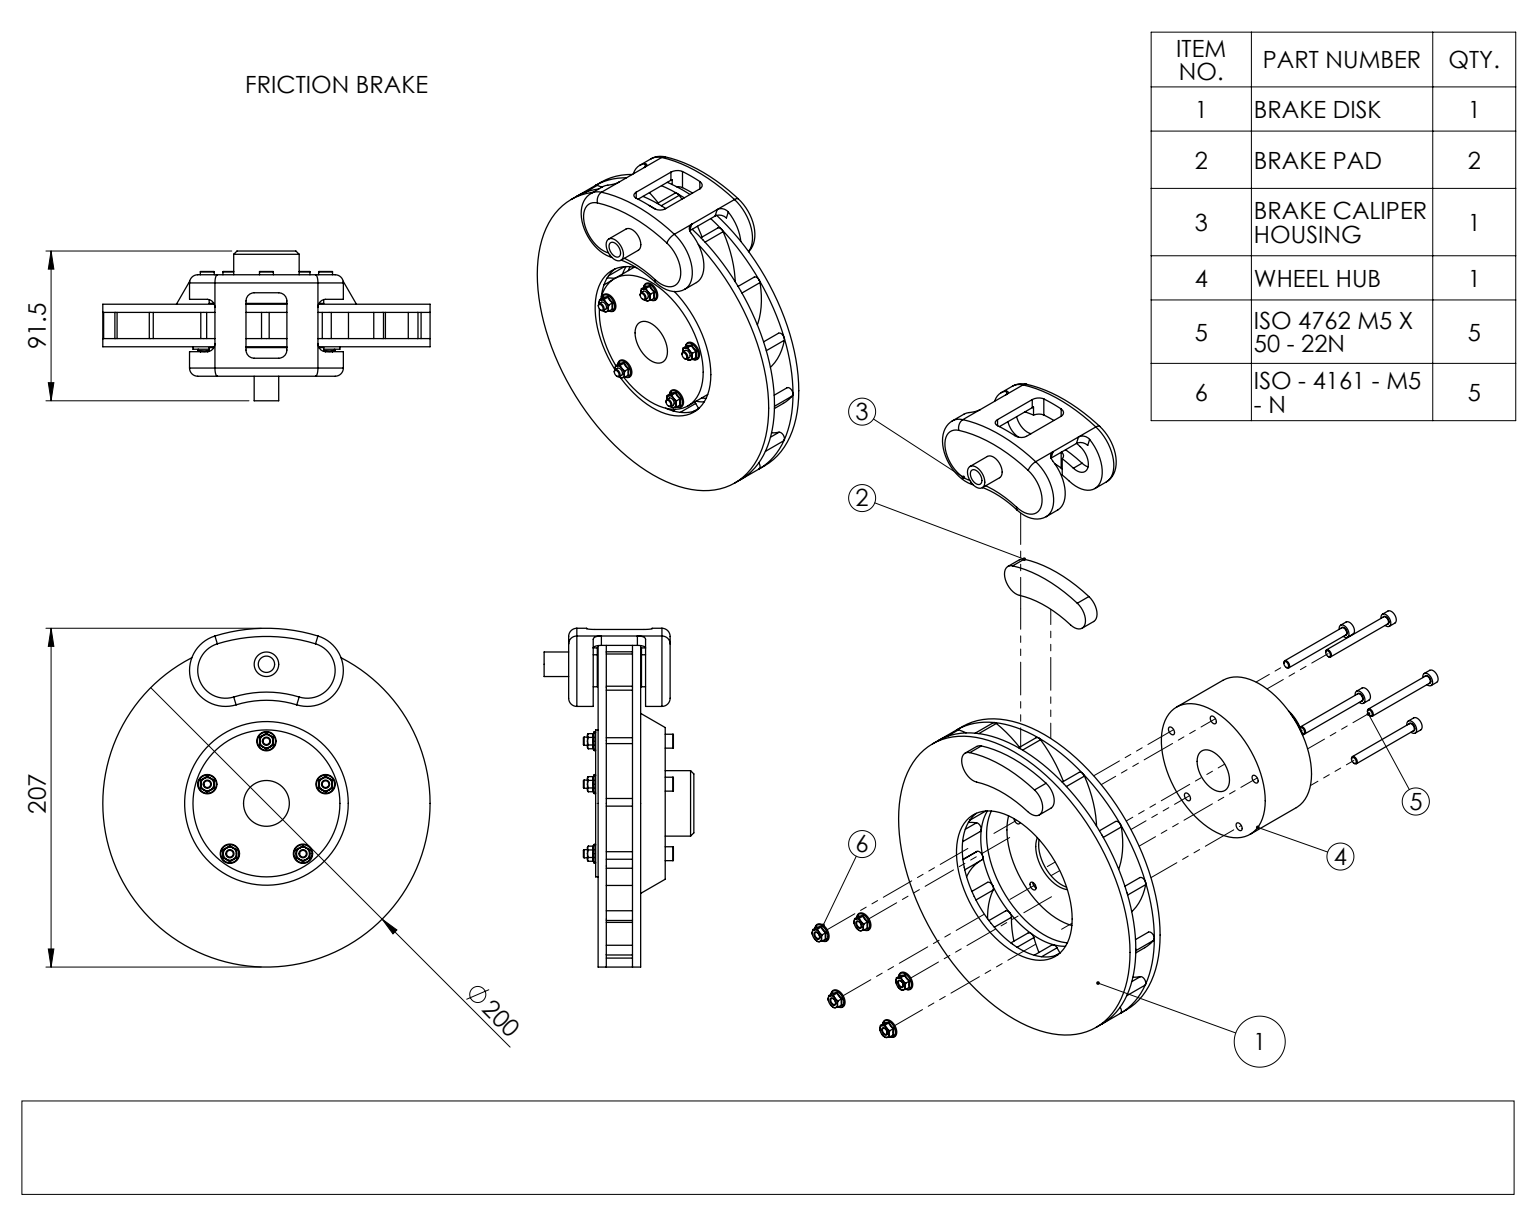
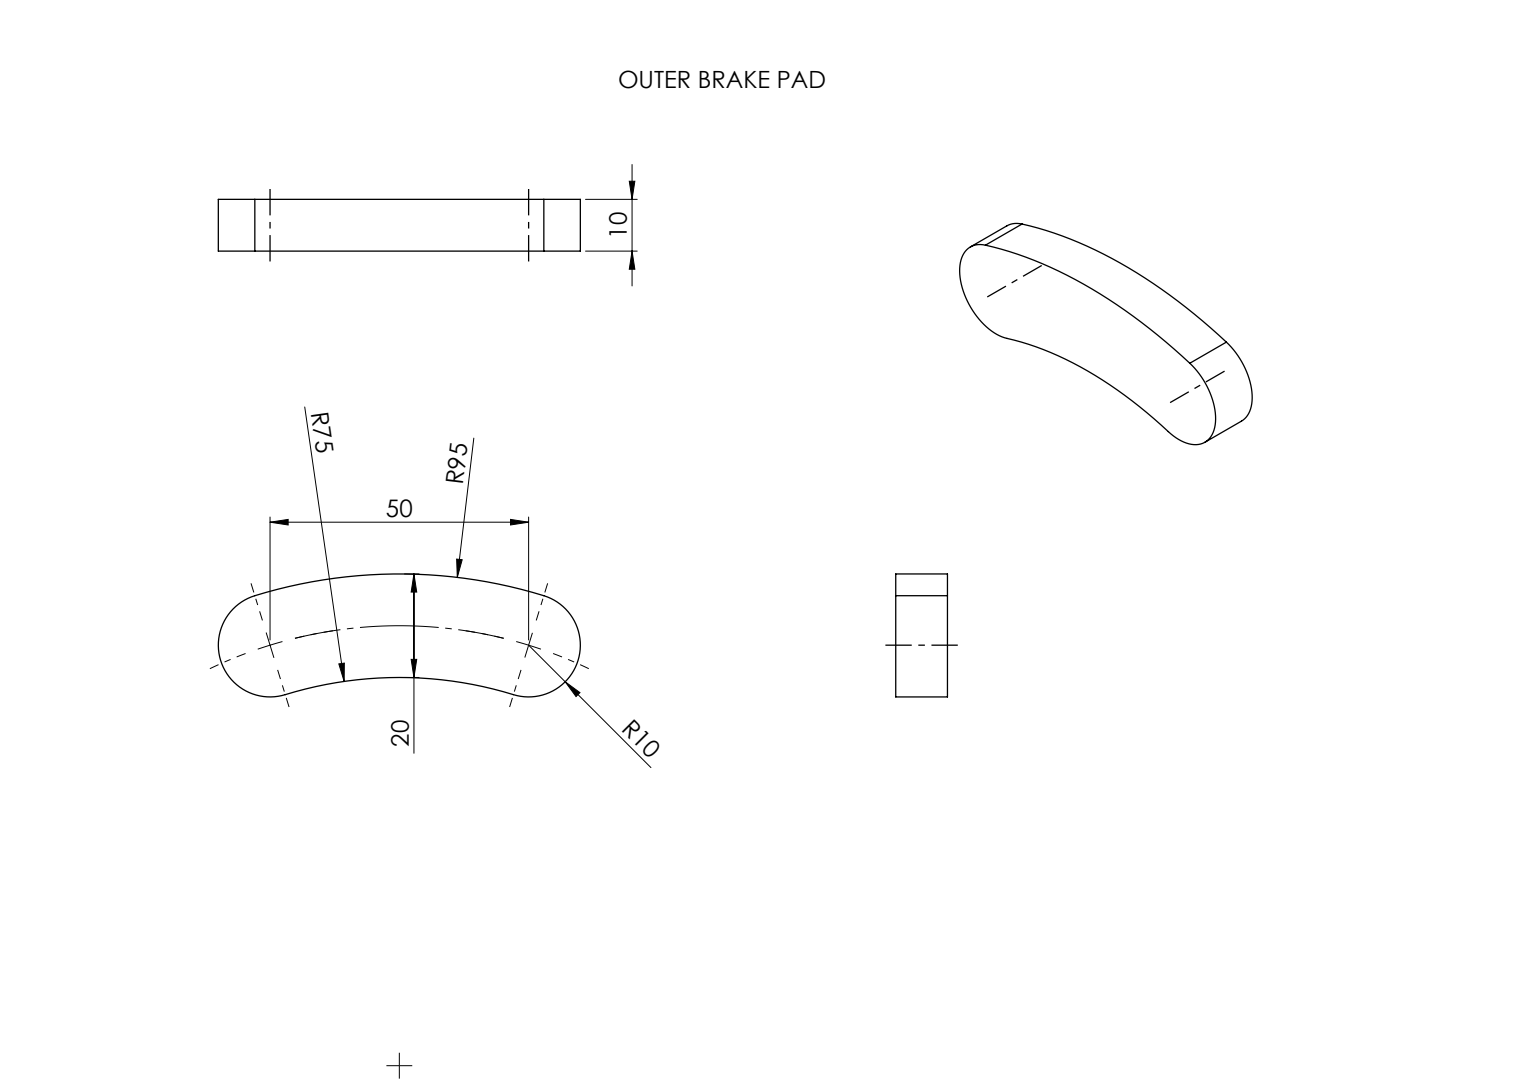
ISO-10303-21;
HEADER;
FILE_DESCRIPTION (('STEP AP214'),
    '1' );
FILE_NAME ('BR-595',
    '2026-10-02T06:35:35',
    ( '' ),
    ( '' ),
    'SwSTEP 2.0',
    'SolidWorks 2026',
    '' );
FILE_SCHEMA (( 'AUTOMOTIVE_DESIGN' ));
ENDSEC;

DATA;
#1 = ORIENTED_EDGE ( 'NONE', *, *, #7352, .F. ) ;
#2 = DIRECTION ( 'NONE',  ( -1.000000000000000000, 0.000000000000000000, 0.000000000000000000 ) ) ;
#3 = DIRECTION ( 'NONE',  ( -1.000000000000000000, 0.000000000000000000, 0.000000000000000000 ) ) ;
#4 = ORIENTED_EDGE ( 'NONE', *, *, #5380, .F. ) ;
#5 = DIRECTION ( 'NONE',  ( -1.000000000000000000, 0.000000000000000000, 0.000000000000000000 ) ) ;
#6 = CIRCLE ( 'NONE', #12861, 63.00000000000000000 ) ;
#7 = CARTESIAN_POINT ( 'NONE',  ( 53.06332297728253877, -7.252293700256950082, -10.50000000000000000 ) ) ;
#8 = FACE_OUTER_BOUND ( 'NONE', #11130, .T. ) ;
#9 = CARTESIAN_POINT ( 'NONE',  ( 2.500000000000002220, -1.178949249685208533, 2.042000000000002036 ) ) ;
#10 = CIRCLE ( 'NONE', #12379, 59.50000000000000711 ) ;
#11 = CARTESIAN_POINT ( 'NONE',  ( 0.000000000000000000, 0.000000000000000000, -10.50000000000000000 ) ) ;
#12 = AXIS2_PLACEMENT_3D ( 'NONE', #10324, #12760, #3495 ) ;
#13 = DIRECTION ( 'NONE',  ( -1.000000000000000000, 0.000000000000000000, 0.000000000000000000 ) ) ;
#14 = VERTEX_POINT ( 'NONE', #5600 ) ;
#15 = AXIS2_PLACEMENT_3D ( 'NONE', #1974, #14669, #772 ) ;
#16 = CARTESIAN_POINT ( 'NONE',  ( -9.706953719245875689, -57.06275842387046993, 10.49999999999999822 ) ) ;
#17 = CARTESIAN_POINT ( 'NONE',  ( 54.55500000000000682, 0.000000000000000000, 0.000000000000000000 ) ) ;
#18 = AXIS2_PLACEMENT_3D ( 'NONE', #11160, #14736, #14806 ) ;
#19 = DIRECTION ( 'NONE',  ( 0.000000000000000000, 0.000000000000000000, 1.000000000000000000 ) ) ;
#20 = CIRCLE ( 'NONE', #4639, 50.00000000000000000 ) ;
#21 = CARTESIAN_POINT ( 'NONE',  ( -3.999999999999996447, 0.000000000000000000, 0.000000000000000000 ) ) ;
#22 = AXIS2_PLACEMENT_3D ( 'NONE', #10002, #1881, #9007 ) ;
#23 = VERTEX_POINT ( 'NONE', #4041 ) ;
#24 = ADVANCED_FACE ( 'NONE', ( #13370 ), #10311, .T. ) ;
#25 = CARTESIAN_POINT ( 'NONE',  ( -57.06275842387042729, 9.706953719246069312, 10.49999999999999822 ) ) ;
#26 = ADVANCED_FACE ( 'NONE', ( #7589 ), #2370, .T. ) ;
#27 = VERTEX_POINT ( 'NONE', #8027 ) ;
#28 = CARTESIAN_POINT ( 'NONE',  ( 0.000000000000000000, 0.000000000000000000, -43.49999999999998579 ) ) ;
#29 = DIRECTION ( 'NONE',  ( 1.000000000000000000, 0.000000000000000000, 0.000000000000000000 ) ) ;
#30 = AXIS2_PLACEMENT_3D ( 'NONE', #3946, #7114, #5981 ) ;
#31 = DIRECTION ( 'NONE',  ( 1.000000000000000000, 0.000000000000000000, 0.000000000000000000 ) ) ;
#32 = DIRECTION ( 'NONE',  ( -1.000000000000000000, 0.000000000000000000, 0.000000000000000000 ) ) ;
#33 = AXIS2_PLACEMENT_3D ( 'NONE', #14453, #639, #4058 ) ;
#34 = EDGE_LOOP ( 'NONE', ( #1936, #8130, #14973, #10499, #11470, #9709, #14107 ) ) ;
#35 = AXIS2_PLACEMENT_3D ( 'NONE', #9136, #13779, #7988 ) ;
#36 = DIRECTION ( 'NONE',  ( -0.000000000000000000, -0.000000000000000000, -1.000000000000000000 ) ) ;
#37 = CYLINDRICAL_SURFACE ( 'NONE', #355, 22.00000000000001421 ) ;
#38 = DIRECTION ( 'NONE',  ( -0.000000000000000000, -0.000000000000000000, -1.000000000000000000 ) ) ;
#39 = ORIENTED_EDGE ( 'NONE', *, *, #13925, .F. ) ;
#40 = AXIS2_PLACEMENT_3D ( 'NONE', #3441, #1165, #12924 ) ;
#41 = EDGE_LOOP ( 'NONE', ( #8481, #11440, #8445, #13506, #14760, #3452, #6224, #9398, #1796 ) ) ;
#42 = EDGE_CURVE ( 'NONE', #5654, #12729, #7938, .T. ) ;
#43 = EDGE_CURVE ( 'NONE', #8906, #2094, #9864, .T. ) ;
#44 = ORIENTED_EDGE ( 'NONE', *, *, #3478, .T. ) ;
#45 = AXIS2_PLACEMENT_3D ( 'NONE', #573, #4845, #14470 ) ;
#46 = CYLINDRICAL_SURFACE ( 'NONE', #4967, 3.000000000000002665 ) ;
#47 = CARTESIAN_POINT ( 'NONE',  ( 47.00000000000001421, 81.24038404635960831, -31.00000000000000000 ) ) ;
#48 = FACE_BOUND ( 'NONE', #7708, .T. ) ;
#49 = CARTESIAN_POINT ( 'NONE',  ( 36.14014761921570340, 11.74264578624841171, -25.50000000000000355 ) ) ;
#50 = DIRECTION ( 'NONE',  ( 0.000000000000000000, 0.000000000000000000, 1.000000000000000000 ) ) ;
#51 = EDGE_LOOP ( 'NONE', ( #11368, #1318, #14890, #12577, #3403 ) ) ;
#52 = CARTESIAN_POINT ( 'NONE',  ( 36.08010649850015739, 100.2464683348682541, -16.00000000000000000 ) ) ;
#53 = DIRECTION ( 'NONE',  ( 1.000000000000000000, 0.000000000000000000, 0.000000000000000000 ) ) ;
#54 = AXIS2_PLACEMENT_3D ( 'NONE', #13528, #11036, #940 ) ;
#55 = ORIENTED_EDGE ( 'NONE', *, *, #8567, .F. ) ;
#56 = ORIENTED_EDGE ( 'NONE', *, *, #8508, .F. ) ;
#57 = DIRECTION ( 'NONE',  ( 0.000000000000000000, 0.000000000000000000, 1.000000000000000000 ) ) ;
#58 = ORIENTED_EDGE ( 'NONE', *, *, #13027, .F. ) ;
#59 = AXIS2_PLACEMENT_3D ( 'NONE', #11530, #114, #4460 ) ;
#60 = CARTESIAN_POINT ( 'NONE',  ( -69.16568774265545017, 71.53347797788843820, -13.00000000000000178 ) ) ;
#61 = CARTESIAN_POINT ( 'NONE',  ( 0.000000000000000000, 0.000000000000000000, -10.50000000000000000 ) ) ;
#62 = EDGE_CURVE ( 'NONE', #7405, #1485, #13775, .T. ) ;
#63 = AXIS2_PLACEMENT_3D ( 'NONE', #8204, #12550, #5924 ) ;
#64 = CARTESIAN_POINT ( 'NONE',  ( 0.000000000000000000, 4.618802153517009401, -0.5000000000000004441 ) ) ;
#65 = CARTESIAN_POINT ( 'NONE',  ( 0.000000000000000000, 0.000000000000000000, -13.00000000000000178 ) ) ;
#66 = VECTOR ( 'NONE', #7777, 1000.000000000000000 ) ;
#67 = CARTESIAN_POINT ( 'NONE',  ( 66.70695371924546180, 57.06275842387054098, 8.000000000000000000 ) ) ;
#68 = CARTESIAN_POINT ( 'NONE',  ( 50.84834283436990177, 14.07862063237912054, -13.00000000000000178 ) ) ;
#69 = ADVANCED_FACE ( 'NONE', ( #14874 ), #12670, .F. ) ;
#70 = ORIENTED_EDGE ( 'NONE', *, *, #7162, .T. ) ;
#71 = CARTESIAN_POINT ( 'NONE',  ( 0.000000000000000000, 4.618802153517009401, -3.433295621305381573 ) ) ;
#72 = AXIS2_PLACEMENT_3D ( 'NONE', #14916, #10416, #5859 ) ;
#73 = EDGE_CURVE ( 'NONE', #4839, #9064, #14954, .T. ) ;
#74 = LINE ( 'NONE', #12542, #3120 ) ;
#75 = ORIENTED_EDGE ( 'NONE', *, *, #14051, .F. ) ;
#76 = FILL_AREA_STYLE ('',( #3580 ) ) ;
#77 = AXIS2_PLACEMENT_3D ( 'NONE', #3248, #7868, #12355 ) ;
#78 = DIRECTION ( 'NONE',  ( 1.000000000000000000, 0.000000000000000000, 0.000000000000000000 ) ) ;
#79 = EDGE_LOOP ( 'NONE', ( #12586, #8672, #6412, #11812, #13520, #7331 ) ) ;
#80 = CYLINDRICAL_SURFACE ( 'NONE', #13351, 59.50000000000000000 ) ;
#81 = EDGE_CURVE ( 'NONE', #7416, #8383, #7204, .T. ) ;
#82 = CIRCLE ( 'NONE', #4216, 63.00000000000000000 ) ;
#83 = EDGE_CURVE ( 'NONE', #7502, #10004, #12318, .T. ) ;
#84 = DIRECTION ( 'NONE',  ( 0.000000000000000000, 0.000000000000000000, 1.000000000000000000 ) ) ;
#85 = CYLINDRICAL_SURFACE ( 'NONE', #14315, 56.99999999999999289 ) ;
#86 = LINE ( 'NONE', #9270, #8545 ) ;
#87 = CARTESIAN_POINT ( 'NONE',  ( -3.999999999999999112, 2.471528634177587946, -3.686887442155188932 ) ) ;
#88 = FACE_OUTER_BOUND ( 'NONE', #3167, .T. ) ;
#89 = CIRCLE ( 'NONE', #12700, 0.2000000000000000944 ) ;
#90 = ORIENTED_EDGE ( 'NONE', *, *, #1930, .F. ) ;
#91 = EDGE_CURVE ( 'NONE', #7570, #11525, #4401, .T. ) ;
#92 = CARTESIAN_POINT ( 'NONE',  ( -10.00610186947451474, 106.5314655734664910, -19.33904518629106306 ) ) ;
#93 = CARTESIAN_POINT ( 'NONE',  ( -2.344047193898592063, -3.265465875126478679, -8.534280460060699911E-15 ) ) ;
#94 = B_SPLINE_CURVE_WITH_KNOTS ( 'NONE', 3,
 ( #9442, #2468, #4910, #4826, #14091, #9801, #11106, #8665, #3618, #8738, #13380, #3696, #12955, #2552, #2981, #7235, #10661, #9522, #3776, #4761 ),
 .UNSPECIFIED., .F., .F.,
 ( 4, 2, 2, 2, 2, 2, 2, 2, 2, 4 ),
 ( 0.000000000000000000, 0.0009783709435495714819, 0.001467556415324351151, 0.001956741887099130821, 0.002935112830648695798, 0.003913483774198260774, 0.004891854717747825751, 0.005870225661297390728, 0.006848596604846954837, 0.007826967548396519814 ),
 .UNSPECIFIED. ) ;
#95 = DIRECTION ( 'NONE',  ( 1.000000000000000000, 0.000000000000000000, 0.000000000000000000 ) ) ;
#96 = DIRECTION ( 'NONE',  ( 0.000000000000000000, 0.000000000000000000, -1.000000000000000000 ) ) ;
#97 = ORIENTED_EDGE ( 'NONE', *, *, #2089, .T. ) ;
#98 = CIRCLE ( 'NONE', #1556, 2.649999999999992806 ) ;
#99 = AXIS2_PLACEMENT_3D ( 'NONE', #4932, #13204, #7338 ) ;
#100 = FACE_OUTER_BOUND ( 'NONE', #3263, .T. ) ;
#101 = AXIS2_PLACEMENT_3D ( 'NONE', #2141, #150, #5905 ) ;
#102 = ORIENTED_EDGE ( 'NONE', *, *, #4360, .F. ) ;
#103 = DIRECTION ( 'NONE',  ( -1.000000000000000000, 0.000000000000000000, 0.000000000000000000 ) ) ;
#104 = DIRECTION ( 'NONE',  ( 1.000000000000000000, 0.000000000000000000, 0.000000000000000000 ) ) ;
#105 = PLANE ( 'NONE',  #6564 ) ;
#106 = DIRECTION ( 'NONE',  ( -0.000000000000000000, -0.000000000000000000, 1.000000000000000000 ) ) ;
#107 = VECTOR ( 'NONE', #12064, 1000.000000000000000 ) ;
#108 = EDGE_LOOP ( 'NONE', ( #5288, #10008 ) ) ;
#109 = CIRCLE ( 'NONE', #11524, 3.000000000000004441 ) ;
#110 = AXIS2_PLACEMENT_3D ( 'NONE', #13113, #9527, #4007 ) ;
#111 = DIRECTION ( 'NONE',  ( 1.000000000000000000, 0.000000000000000000, 0.000000000000000000 ) ) ;
#112 = DIRECTION ( 'NONE',  ( 0.000000000000000000, 0.000000000000000000, -1.000000000000000000 ) ) ;
#113 = AXIS2_PLACEMENT_3D ( 'NONE', #5450, #3170, #7481 ) ;
#114 = DIRECTION ( 'NONE',  ( -0.000000000000000000, -0.000000000000000000, -1.000000000000000000 ) ) ;
#115 = ORIENTED_EDGE ( 'NONE', *, *, #13152, .T. ) ;
#116 = ORIENTED_EDGE ( 'NONE', *, *, #9973, .T. ) ;
#117 = STYLED_ITEM ( 'NONE', ( #11100 ), #4169 ) ;
#118 = ORIENTED_EDGE ( 'NONE', *, *, #6384, .T. ) ;
#119 = AXIS2_PLACEMENT_3D ( 'NONE', #2152, #13621, #8984 ) ;
#120 = DIRECTION ( 'NONE',  ( -1.000000000000000000, 0.000000000000000000, 0.000000000000000000 ) ) ;
#121 = AXIS2_PLACEMENT_3D ( 'NONE', #1011, #8960, #6603 ) ;
#122 = FACE_OUTER_BOUND ( 'NONE', #11782, .T. ) ;
#123 = CARTESIAN_POINT ( 'NONE',  ( 2.836893136758667833, 3.208949435746013545, -3.505054077164964976 ) ) ;
#124 = CARTESIAN_POINT ( 'NONE',  ( 7.417888187663120192, 52.54657765281190507, -13.00000000000000178 ) ) ;
#125 = EDGE_CURVE ( 'NONE', #6463, #5657, #11381, .T. ) ;
#126 = ORIENTED_EDGE ( 'NONE', *, *, #9552, .T. ) ;
#127 = CARTESIAN_POINT ( 'NONE',  ( -10.20439220990035345, 94.45068983291282905, 19.21516791372541633 ) ) ;
#128 = ORIENTED_EDGE ( 'NONE', *, *, #10022, .F. ) ;
#129 = ADVANCED_FACE ( 'NONE', ( #13654 ), #8723, .F. ) ;
#130 = ORIENTED_EDGE ( 'NONE', *, *, #424, .F. ) ;
#131 = EDGE_CURVE ( 'NONE', #9943, #5635, #9786, .T. ) ;
#132 = VERTEX_POINT ( 'NONE', #14438 ) ;
#133 = EDGE_CURVE ( 'NONE', #4919, #1677, #14989, .T. ) ;
#134 = CARTESIAN_POINT ( 'NONE',  ( 4.154306624730861763, 2.398490048084776394, -3.721999068284301604 ) ) ;
#135 = CARTESIAN_POINT ( 'NONE',  ( 12.50000000000000000, 40.62019202317980415, -16.00000000000000000 ) ) ;
#136 = CIRCLE ( 'NONE', #11783, 63.00000000000000000 ) ;
#137 = CARTESIAN_POINT ( 'NONE',  ( 10.21169758550232309, 62.16852661215632025, 19.23993411931846254 ) ) ;
#138 = ORIENTED_EDGE ( 'NONE', *, *, #8514, .T. ) ;
#139 = CIRCLE ( 'NONE', #6147, 3.000000000000002665 ) ;
#140 = EDGE_LOOP ( 'NONE', ( #7272, #903, #5586, #9223, #6785, #6818 ) ) ;
#141 = DIRECTION ( 'NONE',  ( -0.000000000000000000, -0.000000000000000000, -1.000000000000000000 ) ) ;
#142 = EDGE_CURVE ( 'NONE', #2335, #4523, #8651, .T. ) ;
#143 = VERTEX_POINT ( 'NONE', #12163 ) ;
#144 = VECTOR ( 'NONE', #4829, 1000.000000000000000 ) ;
#145 = DIRECTION ( 'NONE',  ( -0.000000000000000000, -0.000000000000000000, 1.000000000000000000 ) ) ;
#146 = DIRECTION ( 'NONE',  ( -1.000000000000000000, 0.000000000000000000, 0.000000000000000000 ) ) ;
#147 = CIRCLE ( 'NONE', #10081, 0.5000000000000004441 ) ;
#148 = DIRECTION ( 'NONE',  ( 1.000000000000000000, 0.000000000000000000, 0.000000000000000000 ) ) ;
#149 = SURFACE_STYLE_FILL_AREA ( #5069 ) ;
#150 = DIRECTION ( 'NONE',  ( -0.000000000000000000, -0.000000000000000000, 1.000000000000000000 ) ) ;
#151 = DIRECTION ( 'NONE',  ( 0.000000000000000000, 0.000000000000000000, 1.000000000000000000 ) ) ;
#152 = ORIENTED_EDGE ( 'NONE', *, *, #3887, .F. ) ;
#153 = DIRECTION ( 'NONE',  ( -1.000000000000000000, 0.000000000000000000, 0.000000000000000000 ) ) ;
#154 = CIRCLE ( 'NONE', #13005, 2.649999999999985700 ) ;
#155 = ADVANCED_FACE ( 'NONE', ( #11017 ), #623, .F. ) ;
#156 = ORIENTED_EDGE ( 'NONE', *, *, #4969, .T. ) ;
#157 =( NAMED_UNIT ( * ) SI_UNIT ( $, .STERADIAN. ) SOLID_ANGLE_UNIT ( ) );
#158 = ORIENTED_EDGE ( 'NONE', *, *, #13672, .T. ) ;
#159 = CARTESIAN_POINT ( 'NONE',  ( 2.500000000000002220, 0.000000000000000000, 0.000000000000000000 ) ) ;
#160 = ORIENTED_EDGE ( 'NONE', *, *, #4028, .F. ) ;
#161 = CARTESIAN_POINT ( 'NONE',  ( 2.500000000000002220, -1.178949249685208533, 2.042000000000002036 ) ) ;
#162 = CARTESIAN_POINT ( 'NONE',  ( -52.72775723226775568, 7.383907457638128058, -13.00000000000000178 ) ) ;
#163 = DIRECTION ( 'NONE',  ( 1.000000000000000000, 0.000000000000000000, 0.000000000000000000 ) ) ;
#164 = CARTESIAN_POINT ( 'NONE',  ( -53.63365512954686665, 9.714003807514082212, 8.000000000000000000 ) ) ;
#165 = AXIS2_PLACEMENT_3D ( 'NONE', #7612, #12181, #14531 ) ;
#166 = DIRECTION ( 'NONE',  ( -0.000000000000000000, -0.000000000000000000, -1.000000000000000000 ) ) ;
#167 = CARTESIAN_POINT ( 'NONE',  ( 36.14014761921570340, 11.74264578624841171, -28.00000000000000000 ) ) ;
#168 = ORIENTED_EDGE ( 'NONE', *, *, #2760, .F. ) ;
#169 = CARTESIAN_POINT ( 'NONE',  ( 0.000000000000000000, 0.000000000000000000, -10.50000000000000000 ) ) ;
#170 = DIRECTION ( 'NONE',  ( 1.000000000000000000, 0.000000000000000000, 0.000000000000000000 ) ) ;
#171 = EDGE_CURVE ( 'NONE', #8488, #2518, #8671, .T. ) ;
#172 = EDGE_CURVE ( 'NONE', #8464, #345, #2401, .T. ) ;
#173 = FACE_OUTER_BOUND ( 'NONE', #9202, .T. ) ;
#174 = CARTESIAN_POINT ( 'NONE',  ( 33.48561063518626923, -47.21331623427104063, 10.49999999999999822 ) ) ;
#175 = ORIENTED_EDGE ( 'NONE', *, *, #2159, .T. ) ;
#176 = CARTESIAN_POINT ( 'NONE',  ( -45.96504489225991819, 23.50071946824089153, -8.000000000000000000 ) ) ;
#177 = ORIENTED_EDGE ( 'NONE', *, *, #5197, .F. ) ;
#178 = DIRECTION ( 'NONE',  ( 1.000000000000000000, 0.000000000000000000, -0.000000000000000000 ) ) ;
#179 = CARTESIAN_POINT ( 'NONE',  ( 35.00000000000000000, 81.24038404635960831, 16.00000000000000000 ) ) ;
#180 = EDGE_CURVE ( 'NONE', #2333, #2935, #11831, .T. ) ;
#181 = CARTESIAN_POINT ( 'NONE',  ( 70.71067811865488295, 70.71067811865464137, 8.000000000000000000 ) ) ;
#182 = DIRECTION ( 'NONE',  ( -0.000000000000000000, -0.000000000000000000, -1.000000000000000000 ) ) ;
#183 = ORIENTED_EDGE ( 'NONE', *, *, #10022, .T. ) ;
#184 = PLANE ( 'NONE',  #4038 ) ;
#185 = DIRECTION ( 'NONE',  ( 1.000000000000000000, 0.000000000000000000, 0.000000000000000000 ) ) ;
#186 = ADVANCED_FACE ( 'NONE', ( #285 ), #5969, .F. ) ;
#187 = DIRECTION ( 'NONE',  ( 0.000000000000000000, 0.000000000000000000, -1.000000000000000000 ) ) ;
#188 = ORIENTED_EDGE ( 'NONE', *, *, #4452, .F. ) ;
#189 = ORIENTED_EDGE ( 'NONE', *, *, #647, .F. ) ;
#190 = ORIENTED_EDGE ( 'NONE', *, *, #13352, .T. ) ;
#191 = DIRECTION ( 'NONE',  ( -0.000000000000000000, -0.000000000000000000, -1.000000000000000000 ) ) ;
#192 = DIRECTION ( 'NONE',  ( -0.000000000000000000, -0.000000000000000000, 1.000000000000000000 ) ) ;
#193 = DIRECTION ( 'NONE',  ( 0.000000000000000000, 0.000000000000000000, 1.000000000000000000 ) ) ;
#194 = SURFACE_SIDE_STYLE ('',( #3699 ) ) ;
#195 = CARTESIAN_POINT ( 'NONE',  ( 92.61631465359491244, 37.12029293941346708, -13.00000000000000178 ) ) ;
#196 = ORIENTED_EDGE ( 'NONE', *, *, #12416, .F. ) ;
#197 = VERTEX_POINT ( 'NONE', #8248 ) ;
#198 = VERTEX_POINT ( 'NONE', #2479 ) ;
#199 = CARTESIAN_POINT ( 'NONE',  ( 43.30127018922200222, -24.99999999999988276, -8.000000000000000000 ) ) ;
#200 = DIRECTION ( 'NONE',  ( 0.000000000000000000, 0.000000000000000000, -1.000000000000000000 ) ) ;
#201 = CARTESIAN_POINT ( 'NONE',  ( 11.10302805179279240, 62.01554028455485224, 18.51404809149990882 ) ) ;
#202 = ORIENTED_EDGE ( 'NONE', *, *, #1757, .T. ) ;
#203 = VERTEX_POINT ( 'NONE', #9455 ) ;
#204 = DIRECTION ( 'NONE',  ( -0.000000000000000000, -0.000000000000000000, -1.000000000000000000 ) ) ;
#205 = ORIENTED_EDGE ( 'NONE', *, *, #9389, .F. ) ;
#206 = EDGE_CURVE ( 'NONE', #7611, #11559, #11845, .T. ) ;
#207 = CARTESIAN_POINT ( 'NONE',  ( -57.06275842387042729, 9.706953719246069312, -8.000000000000000000 ) ) ;
#208 = DIRECTION ( 'NONE',  ( -1.000000000000000000, 0.000000000000000000, 0.000000000000000000 ) ) ;
#209 = ADVANCED_FACE ( 'NONE', ( #8178 ), #13040, .T. ) ;
#210 = CARTESIAN_POINT ( 'NONE',  ( 0.2500000000000002220, 0.000000000000000000, 4.250000000000000000 ) ) ;
#211 = DIRECTION ( 'NONE',  ( 0.000000000000000000, 0.000000000000000000, -1.000000000000000000 ) ) ;
#212 = VERTEX_POINT ( 'NONE', #10456 ) ;
#213 = LINE ( 'NONE', #4355, #3743 ) ;
#214 = CARTESIAN_POINT ( 'NONE',  ( -89.89283556784485540, 37.53686968382331202, 10.49999999999999822 ) ) ;
#215 = VERTEX_POINT ( 'NONE', #4771 ) ;
#216 = DIRECTION ( 'NONE',  ( 0.000000000000000000, 1.000000000000000000, 0.000000000000000000 ) ) ;
#217 = ORIENTED_EDGE ( 'NONE', *, *, #892, .F. ) ;
#218 = VERTEX_POINT ( 'NONE', #1279 ) ;
#219 = VERTEX_POINT ( 'NONE', #12746 ) ;
#220 = ADVANCED_FACE ( 'NONE', ( #7246 ), #8324, .F. ) ;
#221 = DIRECTION ( 'NONE',  ( 0.000000000000000000, 0.000000000000000000, -1.000000000000000000 ) ) ;
#222 = AXIS2_PLACEMENT_3D ( 'NONE', #233, #10789, #392 ) ;
#223 = CARTESIAN_POINT ( 'NONE',  ( 25.00000000000000000, 81.24038404635960831, 26.00000000000000000 ) ) ;
#224 = EDGE_LOOP ( 'NONE', ( #11298, #11985, #10533, #2386, #7022, #5370 ) ) ;
#225 = EDGE_CURVE ( 'NONE', #11976, #1441, #7021, .T. ) ;
#226 = ORIENTED_EDGE ( 'NONE', *, *, #3230, .T. ) ;
#227 = CARTESIAN_POINT ( 'NONE',  ( 3.999999999999996447, -2.309401076758518911, -3.433295621305385126 ) ) ;
#228 = CARTESIAN_POINT ( 'NONE',  ( 0.000000000000000000, 0.000000000000000000, 10.50000000000000000 ) ) ;
#229 = DIRECTION ( 'NONE',  ( -0.000000000000000000, -0.000000000000000000, 1.000000000000000000 ) ) ;
#230 = CARTESIAN_POINT ( 'NONE',  ( 12.39897948556635754, 61.76783392443436327, 16.00000000000000000 ) ) ;
#231 = AXIS2_PLACEMENT_3D ( 'NONE', #12118, #6402, #3087 ) ;
#232 = CIRCLE ( 'NONE', #11153, 59.50000000000000000 ) ;
#233 = CARTESIAN_POINT ( 'NONE',  ( 6.917888187663118416, 52.54657765281190507, -13.00000000000000178 ) ) ;
#234 = EDGE_LOOP ( 'NONE', ( #1184, #579, #7849, #6661 ) ) ;
#235 = CIRCLE ( 'NONE', #7737, 3.000000000000002665 ) ;
#236 = DIRECTION ( 'NONE',  ( 0.000000000000000000, 0.000000000000000000, -1.000000000000000000 ) ) ;
#237 = ORIENTED_EDGE ( 'NONE', *, *, #10239, .T. ) ;
#238 = VECTOR ( 'NONE', #6357, 1000.000000000000000 ) ;
#239 = CARTESIAN_POINT ( 'NONE',  ( 0.000000000000000000, 0.000000000000000000, -13.00000000000000178 ) ) ;
#240 = CYLINDRICAL_SURFACE ( 'NONE', #5888, 0.5000000000000004441 ) ;
#241 = DIRECTION ( 'NONE',  ( 0.000000000000000000, 0.000000000000000000, 1.000000000000000000 ) ) ;
#242 = AXIS2_PLACEMENT_3D ( 'NONE', #11255, #4428, #1840 ) ;
#243 = B_SPLINE_CURVE_WITH_KNOTS ( 'NONE', 3,
 ( #4332, #3259, #11468, #1065, #15025, #13745 ),
 .UNSPECIFIED., .F., .F.,
 ( 4, 2, 4 ),
 ( -3.640115492410820263E-06, 0.0002066546034003392330, 0.0004169493222930892523 ),
 .UNSPECIFIED. ) ;
#244 = DIRECTION ( 'NONE',  ( 0.000000000000000000, 0.000000000000000000, 1.000000000000000000 ) ) ;
#245 = EDGE_LOOP ( 'NONE', ( #12911, #1425, #6697, #4365 ) ) ;
#246 = VECTOR ( 'NONE', #11341, 1000.000000000000000 ) ;
#247 = CARTESIAN_POINT ( 'NONE',  ( 0.000000000000000000, 0.000000000000000000, -13.00000000000000178 ) ) ;
#248 = AXIS2_PLACEMENT_3D ( 'NONE', #2313, #11658, #11591 ) ;
#249 = EDGE_LOOP ( 'NONE', ( #12812, #11025, #8242, #14279, #562, #14719, #2020, #11276, #2397 ) ) ;
#250 = DIRECTION ( 'NONE',  ( -0.000000000000000000, -0.000000000000000000, 1.000000000000000000 ) ) ;
#251 = DIRECTION ( 'NONE',  ( 0.000000000000000000, 0.000000000000000000, -1.000000000000000000 ) ) ;
#252 = EDGE_CURVE ( 'NONE', #915, #5997, #13054, .T. ) ;
#253 = FACE_OUTER_BOUND ( 'NONE', #11246, .T. ) ;
#254 = EDGE_CURVE ( 'NONE', #13058, #12937, #12889, .T. ) ;
#255 = DIRECTION ( 'NONE',  ( 0.000000000000000000, 0.000000000000000000, -1.000000000000000000 ) ) ;
#256 = CIRCLE ( 'NONE', #11911, 100.0000000000000000 ) ;
#257 = AXIS2_PLACEMENT_3D ( 'NONE', #4931, #14259, #10909 ) ;
#258 = ORIENTED_EDGE ( 'NONE', *, *, #4361, .T. ) ;
#259 = VERTEX_POINT ( 'NONE', #10384 ) ;
#260 = PLANE ( 'NONE',  #2332 ) ;
#261 = VECTOR ( 'NONE', #10408, 1000.000000000000000 ) ;
#262 = LINE ( 'NONE', #9512, #1094 ) ;
#263 = AXIS2_PLACEMENT_3D ( 'NONE', #3425, #1153, #13759 ) ;
#264 = CIRCLE ( 'NONE', #5603, 100.0000000000000000 ) ;
#265 = CARTESIAN_POINT ( 'NONE',  ( 2.500000000000002220, -2.357898499370437939, 0.000000000000000000 ) ) ;
#266 = EDGE_CURVE ( 'NONE', #4701, #13246, #688, .T. ) ;
#267 = ORIENTED_EDGE ( 'NONE', *, *, #14506, .F. ) ;
#268 = AXIS2_PLACEMENT_3D ( 'NONE', #7487, #1663, #9475 ) ;
#269 = ORIENTED_EDGE ( 'NONE', *, *, #1652, .T. ) ;
#270 = AXIS2_PLACEMENT_3D ( 'NONE', #9018, #6504, #12227 ) ;
#271 = DIRECTION ( 'NONE',  ( -0.000000000000000000, -0.000000000000000000, 1.000000000000000000 ) ) ;
#272 = AXIS2_PLACEMENT_3D ( 'NONE', #7169, #13184, #425 ) ;
#273 = EDGE_CURVE ( 'NONE', #3532, #8404, #4570, .T. ) ;
#274 = FACE_BOUND ( 'NONE', #10845, .T. ) ;
#275 = EDGE_CURVE ( 'NONE', #7416, #12316, #7948, .T. ) ;
#276 = AXIS2_PLACEMENT_3D ( 'NONE', #8832, #3149, #952 ) ;
#277 = CARTESIAN_POINT ( 'NONE',  ( 0.000000000000000000, -2.357898499370437939, 0.000000000000000000 ) ) ;
#278 =( LENGTH_UNIT ( ) NAMED_UNIT ( * ) SI_UNIT ( .MILLI., .METRE. ) );
#279 = CYLINDRICAL_SURFACE ( 'NONE', #11305, 0.5000000000000004441 ) ;
#280 = ORIENTED_EDGE ( 'NONE', *, *, #6420, .T. ) ;
#281 = ORIENTED_EDGE ( 'NONE', *, *, #10347, .F. ) ;
#282 = ORIENTED_EDGE ( 'NONE', *, *, #7023, .T. ) ;
#283 = ORIENTED_EDGE ( 'NONE', *, *, #14608, .F. ) ;
#284 = CARTESIAN_POINT ( 'NONE',  ( -9.706953719245875689, -57.06275842387046993, -8.000000000000000000 ) ) ;
#285 = FACE_OUTER_BOUND ( 'NONE', #6940, .T. ) ;
#286 = CIRCLE ( 'NONE', #8760, 2.649999999999985700 ) ;
#287 = CARTESIAN_POINT ( 'NONE',  ( -42.04772703543551415, -32.26435573746212526, 8.000000000000000000 ) ) ;
#288 = EDGE_LOOP ( 'NONE', ( #5939, #663, #3564, #6991, #11925, #8225 ) ) ;
#289 = CIRCLE ( 'NONE', #11702, 2.649999999999985700 ) ;
#290 = ORIENTED_EDGE ( 'NONE', *, *, #1074, .T. ) ;
#291 = DIRECTION ( 'NONE',  ( -0.000000000000000000, -0.000000000000000000, 1.000000000000000000 ) ) ;
#292 = EDGE_LOOP ( 'NONE', ( #2950, #14683, #2755, #9795, #13525 ) ) ;
#293 = DIRECTION ( 'NONE',  ( 0.000000000000000000, 0.000000000000000000, -1.000000000000000000 ) ) ;
#294 = VECTOR ( 'NONE', #9965, 1000.000000000000000 ) ;
#295 = DIRECTION ( 'NONE',  ( 0.000000000000000000, 0.000000000000000000, -1.000000000000000000 ) ) ;
#296 = CARTESIAN_POINT ( 'NONE',  ( 0.000000000000000000, 0.000000000000000000, 0.000000000000000000 ) ) ;
#297 = VERTEX_POINT ( 'NONE', #3559 ) ;
#298 = FACE_OUTER_BOUND ( 'NONE', #14007, .T. ) ;
#299 = DIRECTION ( 'NONE',  ( 0.000000000000000000, 0.000000000000000000, -1.000000000000000000 ) ) ;
#300 = EDGE_LOOP ( 'NONE', ( #5220, #1476, #5090, #12913, #8527, #13334 ) ) ;
#301 = CYLINDRICAL_SURFACE ( 'NONE', #14086, 3.000000000000004441 ) ;
#302 = EDGE_CURVE ( 'NONE', #8589, #2566, #1412, .T. ) ;
#303 = VERTEX_POINT ( 'NONE', #6955 ) ;
#304 = AXIS2_PLACEMENT_3D ( 'NONE', #341, #1635, #4982 ) ;
#305 = ORIENTED_EDGE ( 'NONE', *, *, #10378, .T. ) ;
#306 = CARTESIAN_POINT ( 'NONE',  ( 2.166671187435639459E-31, -4.618802153517023612, -3.504271511727135024 ) ) ;
#307 = ORIENTED_EDGE ( 'NONE', *, *, #3478, .F. ) ;
#308 = DIRECTION ( 'NONE',  ( 1.000000000000000000, 0.000000000000000000, 0.000000000000000000 ) ) ;
#309 = AXIS2_PLACEMENT_3D ( 'NONE', #3603, #2453, #104 ) ;
#310 = CARTESIAN_POINT ( 'NONE',  ( 34.93100731845030538, 100.8740421756369585, -15.84356320956305986 ) ) ;
#311 = DIRECTION ( 'NONE',  ( -1.000000000000000000, 0.000000000000000000, 0.000000000000000000 ) ) ;
#312 = DIRECTION ( 'NONE',  ( 0.000000000000000000, 0.000000000000000000, 1.000000000000000000 ) ) ;
#313 = CARTESIAN_POINT ( 'NONE',  ( -2.449293598294708880E-16, 38.00000000000000000, -25.50000000000000355 ) ) ;
#314 = CARTESIAN_POINT ( 'NONE',  ( -89.61631465359519666, -37.12029293941281338, 8.000000000000000000 ) ) ;
#315 = AXIS2_PLACEMENT_3D ( 'NONE', #10797, #13156, #2521 ) ;
#316 = ORIENTED_EDGE ( 'NONE', *, *, #9761, .T. ) ;
#317 = FACE_OUTER_BOUND ( 'NONE', #3117, .T. ) ;
#318 = CIRCLE ( 'NONE', #5648, 59.50000000000000000 ) ;
#319 = ORIENTED_EDGE ( 'NONE', *, *, #3102, .F. ) ;
#320 = ADVANCED_FACE ( 'NONE', ( #5891 ), #10531, .F. ) ;
#321 = EDGE_CURVE ( 'NONE', #8628, #10615, #10617, .T. ) ;
#322 = ADVANCED_FACE ( 'NONE', ( #2789 ), #4156, .F. ) ;
#323 = CARTESIAN_POINT ( 'NONE',  ( -9.716053034936795285, 106.5583837859906424, -19.49385781195229228 ) ) ;
#324 = DIRECTION ( 'NONE',  ( -1.000000000000000000, 0.000000000000000000, 0.000000000000000000 ) ) ;
#325 = PLANE ( 'NONE',  #8368 ) ;
#326 = CARTESIAN_POINT ( 'NONE',  ( 31.47058823529413374, 102.2673069760056563, -31.00000000000000000 ) ) ;
#327 = ORIENTED_EDGE ( 'NONE', *, *, #5681, .F. ) ;
#328 = AXIS2_PLACEMENT_3D ( 'NONE', #10103, #12541, #12462 ) ;
#329 = ORIENTED_EDGE ( 'NONE', *, *, #3965, .F. ) ;
#330 = DIRECTION ( 'NONE',  ( 0.000000000000000000, 0.000000000000000000, -1.000000000000000000 ) ) ;
#331 = VERTEX_POINT ( 'NONE', #8544 ) ;
#332 = PLANE ( 'NONE',  #4860 ) ;
#333 = DIRECTION ( 'NONE',  ( 0.000000000000000000, 0.000000000000000000, 1.000000000000000000 ) ) ;
#334 = CIRCLE ( 'NONE', #2033, 56.99999999999999289 ) ;
#335 = CARTESIAN_POINT ( 'NONE',  ( -33.08820577230232374, 101.7009610928537171, -14.78158739605038186 ) ) ;
#336 = CARTESIAN_POINT ( 'NONE',  ( -9.706953719245875689, -57.06275842387046993, -13.00000000000000178 ) ) ;
#337 = VERTEX_POINT ( 'NONE', #667 ) ;
#338 = DIRECTION ( 'NONE',  ( 0.000000000000000000, 0.000000000000000000, 1.000000000000000000 ) ) ;
#339 = DIRECTION ( 'NONE',  ( 0.000000000000000000, 0.000000000000000000, 1.000000000000000000 ) ) ;
#340 = AXIS2_PLACEMENT_3D ( 'NONE', #3361, #10273, #9197 ) ;
#341 = CARTESIAN_POINT ( 'NONE',  ( 25.00000000000000000, 81.24038404635960831, -31.00000000000000000 ) ) ;
#342 = CIRCLE ( 'NONE', #8819, 75.00000000000001421 ) ;
#343 = CIRCLE ( 'NONE', #13938, 3.000000000000002665 ) ;
#344 = EDGE_CURVE ( 'NONE', #7966, #6056, #4085, .T. ) ;
#345 = VERTEX_POINT ( 'NONE', #11064 ) ;
#346 = DIRECTION ( 'NONE',  ( 1.000000000000000000, 0.000000000000000000, 0.000000000000000000 ) ) ;
#347 = ORIENTED_EDGE ( 'NONE', *, *, #12989, .T. ) ;
#348 = EDGE_CURVE ( 'NONE', #6889, #6138, #12080, .T. ) ;
#349 = CARTESIAN_POINT ( 'NONE',  ( 0.000000000000000000, 0.000000000000000000, -4.000000000000000000 ) ) ;
#350 = CARTESIAN_POINT ( 'NONE',  ( 10.43254889841015753, 62.13061131512487378, -19.05984907584257115 ) ) ;
#351 = DIRECTION ( 'NONE',  ( -1.000000000000000000, 0.000000000000000000, 0.000000000000000000 ) ) ;
#352 = DIRECTION ( 'NONE',  ( 0.000000000000000000, 0.000000000000000000, 1.000000000000000000 ) ) ;
#353 = DIRECTION ( 'NONE',  ( 0.000000000000000000, 0.000000000000000000, 1.000000000000000000 ) ) ;
#354 = AXIS2_PLACEMENT_3D ( 'NONE', #14127, #13062, #5918 ) ;
#355 = AXIS2_PLACEMENT_3D ( 'NONE', #4755, #11596, #10653 ) ;
#356 = AXIS2_PLACEMENT_3D ( 'NONE', #3246, #11748, #1413 ) ;
#357 = ORIENTED_EDGE ( 'NONE', *, *, #7968, .F. ) ;
#358 = EDGE_LOOP ( 'NONE', ( #1201, #1005, #6170, #12433, #283 ) ) ;
#359 = DIRECTION ( 'NONE',  ( 0.000000000000000000, 0.000000000000000000, 1.000000000000000000 ) ) ;
#360 = DIRECTION ( 'NONE',  ( -0.000000000000000000, -0.000000000000000000, -1.000000000000000000 ) ) ;
#361 = DIRECTION ( 'NONE',  ( 0.000000000000000000, 0.000000000000000000, 1.000000000000000000 ) ) ;
#362 = VERTEX_POINT ( 'NONE', #7552 ) ;
#363 = EDGE_CURVE ( 'NONE', #10590, #2920, #12567, .T. ) ;
#364 = AXIS2_PLACEMENT_3D ( 'NONE', #5973, #204, #2567 ) ;
#365 = ADVANCED_FACE ( 'NONE', ( #7410 ), #14399, .T. ) ;
#366 = ORIENTED_EDGE ( 'NONE', *, *, #266, .F. ) ;
#367 = CARTESIAN_POINT ( 'NONE',  ( -30.80502811811232888, -49.00442420935981147, -8.000000000000000000 ) ) ;
#368 = CIRCLE ( 'NONE', #4978, 53.55662432702593634 ) ;
#369 = AXIS2_PLACEMENT_3D ( 'NONE', #5329, #6524, #6684 ) ;
#370 = ORIENTED_EDGE ( 'NONE', *, *, #5461, .F. ) ;
#371 = CARTESIAN_POINT ( 'NONE',  ( -9.706953719245875689, -57.06275842387046993, -13.00000000000000178 ) ) ;
#372 = CARTESIAN_POINT ( 'NONE',  ( -4.101948962586058123, -2.368261337751176310, -3.681124513963741851 ) ) ;
#373 = DIRECTION ( 'NONE',  ( 0.000000000000000000, 0.000000000000000000, -1.000000000000000000 ) ) ;
#374 = EDGE_CURVE ( 'NONE', #219, #7084, #3764, .T. ) ;
#375 = EDGE_LOOP ( 'NONE', ( #14396, #4852, #5447, #9385 ) ) ;
#376 = DIRECTION ( 'NONE',  ( 0.000000000000000000, 0.000000000000000000, 1.000000000000000000 ) ) ;
#377 = DIRECTION ( 'NONE',  ( 1.000000000000000000, 0.000000000000000000, 0.000000000000000000 ) ) ;
#378 = ORIENTED_EDGE ( 'NONE', *, *, #11049, .T. ) ;
#379 = DIRECTION ( 'NONE',  ( -0.000000000000000000, -0.000000000000000000, -1.000000000000000000 ) ) ;
#380 = CIRCLE ( 'NONE', #5704, 59.50000000000000000 ) ;
#381 = ORIENTED_EDGE ( 'NONE', *, *, #5819, .F. ) ;
#382 = EDGE_CURVE ( 'NONE', #697, #1597, #12234, .T. ) ;
#383 = ORIENTED_EDGE ( 'NONE', *, *, #10951, .T. ) ;
#384 = CARTESIAN_POINT ( 'NONE',  ( 13.71740939043365337, -51.19406879332061067, -10.50000000000000000 ) ) ;
#385 = AXIS2_PLACEMENT_3D ( 'NONE', #8772, #8688, #3163 ) ;
#386 = CIRCLE ( 'NONE', #14206, 0.5000000000000043299 ) ;
#387 = DIRECTION ( 'NONE',  ( 1.000000000000000000, 9.130123557772668088E-16, 0.000000000000000000 ) ) ;
#388 = CARTESIAN_POINT ( 'NONE',  ( 6.451868917687939131, 52.36539807335604024, -13.00000000000000178 ) ) ;
#389 = DIRECTION ( 'NONE',  ( -1.000000000000000000, 0.000000000000000000, 0.000000000000000000 ) ) ;
#390 = CARTESIAN_POINT ( 'NONE',  ( 0.000000000000000000, 0.000000000000000000, -10.50000000000000000 ) ) ;
#391 = CYLINDRICAL_SURFACE ( 'NONE', #8713, 2.649999999999989253 ) ;
#392 = DIRECTION ( 'NONE',  ( 1.000000000000000000, 0.000000000000000000, 0.000000000000000000 ) ) ;
#393 = ORIENTED_EDGE ( 'NONE', *, *, #11619, .F. ) ;
#394 = AXIS2_PLACEMENT_3D ( 'NONE', #10510, #36, #111 ) ;
#395 = SURFACE_STYLE_USAGE ( .BOTH. , #9567 ) ;
#396 = ORIENTED_EDGE ( 'NONE', *, *, #13309, .T. ) ;
#397 = CARTESIAN_POINT ( 'NONE',  ( -11.83867104060235853, 106.3432143034623749, -17.50653253748098948 ) ) ;
#398 = CYLINDRICAL_SURFACE ( 'NONE', #7576, 44.89637028918153305 ) ;
#399 = DIRECTION ( 'NONE',  ( 1.000000000000000000, 0.000000000000000000, 0.000000000000000000 ) ) ;
#400 = CARTESIAN_POINT ( 'NONE',  ( 26.24999999999972289, 45.46633369868319363, -10.50000000000000000 ) ) ;
#401 = EDGE_LOOP ( 'NONE', ( #4330, #13491, #1579, #14951 ) ) ;
#402 = ORIENTED_EDGE ( 'NONE', *, *, #8056, .F. ) ;
#403 = AXIS2_PLACEMENT_3D ( 'NONE', #16, #4438, #10272 ) ;
#404 = EDGE_CURVE ( 'NONE', #6283, #13552, #12722, .T. ) ;
#405 = CARTESIAN_POINT ( 'NONE',  ( 12.46631608856921325, 100.2277185551817951, 15.67011936326128563 ) ) ;
#406 = VERTEX_POINT ( 'NONE', #4008 ) ;
#407 = CARTESIAN_POINT ( 'NONE',  ( -45.89934640057513349, 26.50000000000019540, 10.49999999999999822 ) ) ;
#408 = EDGE_CURVE ( 'NONE', #8250, #5635, #109, .T. ) ;
#409 = DIRECTION ( 'NONE',  ( 1.000000000000000000, 0.000000000000000000, -0.000000000000000000 ) ) ;
#410 = ADVANCED_FACE ( 'NONE', ( #6410 ), #1721, .F. ) ;
#411 = CARTESIAN_POINT ( 'NONE',  ( -31.71893208106490292, 102.1896529572239700, -12.62523369519216310 ) ) ;
#412 = DIRECTION ( 'NONE',  ( 1.000000000000000000, 0.000000000000000000, 0.000000000000000000 ) ) ;
#413 = FACE_OUTER_BOUND ( 'NONE', #6825, .T. ) ;
#414 = ORIENTED_EDGE ( 'NONE', *, *, #11571, .T. ) ;
#415 = DIRECTION ( 'NONE',  ( 0.000000000000000000, 0.000000000000000000, -1.000000000000000000 ) ) ;
#416 = EDGE_CURVE ( 'NONE', #11469, #12633, #6883, .T. ) ;
#417 = FACE_OUTER_BOUND ( 'NONE', #10979, .T. ) ;
#418 = CARTESIAN_POINT ( 'NONE',  ( -32.06294366074467206, 42.50536573064442081, -13.00000000000000178 ) ) ;
#419 = ORIENTED_EDGE ( 'NONE', *, *, #13917, .T. ) ;
#420 = PRODUCT_DEFINITION ( 'UNKNOWN', '', #3883, #9818 ) ;
#421 = LINE ( 'NONE', #7462, #13600 ) ;
#422 = EDGE_LOOP ( 'NONE', ( #2628, #5228, #14534, #2063, #11947 ) ) ;
#423 = DIRECTION ( 'NONE',  ( -0.000000000000000000, -0.000000000000000000, -1.000000000000000000 ) ) ;
#424 = EDGE_CURVE ( 'NONE', #5520, #12576, #13268, .T. ) ;
#425 = DIRECTION ( 'NONE',  ( 1.000000000000000000, 0.000000000000000000, 0.000000000000000000 ) ) ;
#426 = CARTESIAN_POINT ( 'NONE',  ( 26.49999999999971578, 45.89934640057541060, 8.000000000000000000 ) ) ;
#427 = PRESENTATION_STYLE_ASSIGNMENT (( #6185 ) ) ;
#428 = CARTESIAN_POINT ( 'NONE',  ( -29.82779671029264890, 96.49509599019863515, -12.13403317654896973 ) ) ;
#429 = ORIENTED_EDGE ( 'NONE', *, *, #374, .T. ) ;
#430 = DIRECTION ( 'NONE',  ( 0.000000000000000000, 0.000000000000000000, 1.000000000000000000 ) ) ;
#431 = DIRECTION ( 'NONE',  ( 0.000000000000000000, 0.000000000000000000, 1.000000000000000000 ) ) ;
#432 = LINE ( 'NONE', #14181, #7837 ) ;
#433 = ORIENTED_EDGE ( 'NONE', *, *, #10895, .F. ) ;
#434 = CLOSED_SHELL ( 'NONE', ( #8197, #11127, #13290, #14509, #14180, #5659, #1628, #1611, #1202, #2862, #9335, #12100, #8859, #6336, #14665, #11456, #8232, #5781, #3982, #14557, #1671 ) ) ;
#435 = ORIENTED_EDGE ( 'NONE', *, *, #12207, .T. ) ;
#436 = CARTESIAN_POINT ( 'NONE',  ( -12.86891638962156215, 56.43380494353993271, -13.00000000000000178 ) ) ;
#437 = ORIENTED_EDGE ( 'NONE', *, *, #14604, .T. ) ;
#438 = CARTESIAN_POINT ( 'NONE',  ( 0.000000000000000000, 0.000000000000000000, 3.469446951953614189E-15 ) ) ;
#439 = DIRECTION ( 'NONE',  ( 0.000000000000000000, 0.000000000000000000, 1.000000000000000000 ) ) ;
#440 = FILL_AREA_STYLE_COLOUR ( '', #7271 ) ;
#441 = EDGE_CURVE ( 'NONE', #2510, #5889, #6160, .T. ) ;
#442 = DIRECTION ( 'NONE',  ( 0.000000000000000000, 0.000000000000000000, 1.000000000000000000 ) ) ;
#443 = PLANE ( 'NONE',  #14295 ) ;
#444 = EDGE_CURVE ( 'NONE', #1981, #12602, #7473, .T. ) ;
#445 = ORIENTED_EDGE ( 'NONE', *, *, #12228, .T. ) ;
#446 = DIRECTION ( 'NONE',  ( 1.000000000000000000, 0.000000000000000000, 0.000000000000000000 ) ) ;
#447 = ADVANCED_FACE ( 'NONE', ( #10901 ), #4998, .F. ) ;
#448 = ORIENTED_EDGE ( 'NONE', *, *, #10981, .T. ) ;
#449 = EDGE_LOOP ( 'NONE', ( #13543, #13399, #11232, #10086 ) ) ;
#450 = CARTESIAN_POINT ( 'NONE',  ( -33.23060097332287199, 95.37689352056797532, 15.83317473434553690 ) ) ;
#451 = EDGE_CURVE ( 'NONE', #5954, #7016, #6898, .T. ) ;
#452 = VERTEX_POINT ( 'NONE', #4459 ) ;
#453 = LINE ( 'NONE', #9482, #11663 ) ;
#454 = CARTESIAN_POINT ( 'NONE',  ( 0.2500000000000002220, 0.000000000000000000, 0.000000000000000000 ) ) ;
#455 = DIRECTION ( 'NONE',  ( 0.7071067811865444641, 0.000000000000000000, 0.7071067811865505703 ) ) ;
#456 = CARTESIAN_POINT ( 'NONE',  ( 1.317756351988344177, -3.857995168970210997, -0.04852650426602210521 ) ) ;
#457 = CARTESIAN_POINT ( 'NONE',  ( -1.654252653721913102, -3.663718938583020446, -0.01223254789874216215 ) ) ;
#458 = EDGE_CURVE ( 'NONE', #8255, #4053, #4312, .T. ) ;
#459 = ORIENTED_EDGE ( 'NONE', *, *, #7753, .T. ) ;
#460 =( NAMED_UNIT ( * ) SI_UNIT ( $, .STERADIAN. ) SOLID_ANGLE_UNIT ( ) );
#461 = EDGE_LOOP ( 'NONE', ( #5076, #2101 ) ) ;
#462 = DIRECTION ( 'NONE',  ( 0.000000000000000000, 0.000000000000000000, 1.000000000000000000 ) ) ;
#463 = AXIS2_PLACEMENT_3D ( 'NONE', #9565, #3739, #8433 ) ;
#464 = CARTESIAN_POINT ( 'NONE',  ( -0.2790467552932288098, -97.41488903138106537, -13.00000000000000178 ) ) ;
#465 = ORIENTED_EDGE ( 'NONE', *, *, #515, .F. ) ;
#466 = CYLINDRICAL_SURFACE ( 'NONE', #5882, 0.5000000000000004441 ) ;
#467 = B_SPLINE_CURVE_WITH_KNOTS ( 'NONE', 3,
 ( #4608, #10222, #15012, #14864, #7939, #12736, #1129, #12580, #13880, #3468, #13799, #2170, #3388, #6787, #11451, #12658, #1049, #8088 ),
 .UNSPECIFIED., .F., .F.,
 ( 4, 2, 2, 2, 2, 2, 2, 2, 4 ),
 ( 0.001002962753164633562, 0.001858089309406475969, 0.002713215865648318376, 0.003568342421890161216, 0.004423468978132004056, 0.005278595534373846029, 0.006133722090615688870, 0.006988848646857530843, 0.007843975203099373683 ),
 .UNSPECIFIED. ) ;
#468 = LINE ( 'NONE', #10724, #10763 ) ;
#469 = VERTEX_POINT ( 'NONE', #8918 ) ;
#470 = CARTESIAN_POINT ( 'NONE',  ( 12.50000000000000000, 100.2235002382176248, 15.00000000000000000 ) ) ;
#471 = MECHANICAL_DESIGN_GEOMETRIC_PRESENTATION_REPRESENTATION (  '', ( #9665 ), #12840 ) ;
#472 = ORIENTED_EDGE ( 'NONE', *, *, #3041, .F. ) ;
#473 = DIRECTION ( 'NONE',  ( -1.000000000000000000, 0.000000000000000000, 0.000000000000000000 ) ) ;
#474 = CARTESIAN_POINT ( 'NONE',  ( -4.211140560182194292, -2.431303136016555122, -3.745885042887437510 ) ) ;
#475 = CONICAL_SURFACE ( 'NONE', #1692, 5.560781378645573980, 1.221730476396046816 ) ;
#476 = DIRECTION ( 'NONE',  ( 0.000000000000000000, 0.000000000000000000, 1.000000000000000000 ) ) ;
#477 = CARTESIAN_POINT ( 'NONE',  ( -32.26435573746199736, 42.04772703543562073, -13.00000000000000178 ) ) ;
#478 = DIRECTION ( 'NONE',  ( 0.000000000000000000, 0.000000000000000000, 1.000000000000000000 ) ) ;
#479 = VERTEX_POINT ( 'NONE', #11213 ) ;
#480 = DIRECTION ( 'NONE',  ( 0.000000000000000000, 0.000000000000000000, -1.000000000000000000 ) ) ;
#481 = DIRECTION ( 'NONE',  ( 1.000000000000000000, 0.000000000000000000, 0.000000000000000000 ) ) ;
#482 = CIRCLE ( 'NONE', #5802, 3.000000000000004441 ) ;
#483 = FACE_OUTER_BOUND ( 'NONE', #10528, .T. ) ;
#484 = CIRCLE ( 'NONE', #8961, 53.55662432702593634 ) ;
#485 = EDGE_CURVE ( 'NONE', #13764, #628, #7706, .T. ) ;
#486 = CIRCLE ( 'NONE', #10422, 3.000000000000002665 ) ;
#487 = VECTOR ( 'NONE', #2049, 1000.000000000000000 ) ;
#488 = EDGE_LOOP ( 'NONE', ( #55, #3617, #4993, #56, #14251, #1002 ) ) ;
#489 = DIRECTION ( 'NONE',  ( 0.000000000000000000, 0.000000000000000000, 1.000000000000000000 ) ) ;
#490 = VERTEX_POINT ( 'NONE', #9989 ) ;
#491 = CARTESIAN_POINT ( 'NONE',  ( -50.84834283437000835, -14.07862063237876704, -10.50000000000000000 ) ) ;
#492 = CARTESIAN_POINT ( 'NONE',  ( 6.917888187663118416, 52.54657765281190507, -8.000000000000000000 ) ) ;
#493 = ORIENTED_EDGE ( 'NONE', *, *, #10102, .F. ) ;
#494 = AXIS2_PLACEMENT_3D ( 'NONE', #3812, #6062, #12011 ) ;
#495 = CARTESIAN_POINT ( 'NONE',  ( 11.45661564179884451, 61.94983405580222069, -18.07016506142804246 ) ) ;
#496 = FACE_BOUND ( 'NONE', #15028, .T. ) ;
#497 = CARTESIAN_POINT ( 'NONE',  ( 22.33583958711425765, -30.74264578624780242, 19.49999999999999645 ) ) ;
#498 = DIRECTION ( 'NONE',  ( 0.000000000000000000, 0.000000000000000000, -1.000000000000000000 ) ) ;
#499 = CIRCLE ( 'NONE', #8254, 100.0000000000000000 ) ;
#500 = ORIENTED_EDGE ( 'NONE', *, *, #5316, .T. ) ;
#501 = ORIENTED_EDGE ( 'NONE', *, *, #6565, .F. ) ;
#502 =( GEOMETRIC_REPRESENTATION_CONTEXT ( 3 ) GLOBAL_UNCERTAINTY_ASSIGNED_CONTEXT ( ( #12183 ) ) GLOBAL_UNIT_ASSIGNED_CONTEXT ( ( #14644, #1878, #7565 ) ) REPRESENTATION_CONTEXT ( 'NONE', 'WORKASPACE' ) );
#503 = DIRECTION ( 'NONE',  ( 1.000000000000000000, 0.000000000000000000, 0.000000000000000000 ) ) ;
#504 = DIRECTION ( 'NONE',  ( -1.000000000000000000, 0.000000000000000000, 0.000000000000000000 ) ) ;
#505 = CARTESIAN_POINT ( 'NONE',  ( -39.04772703543551415, -32.26435573746212526, -13.00000000000000178 ) ) ;
#506 = EDGE_CURVE ( 'NONE', #259, #13406, #11535, .T. ) ;
#508 = VERTEX_POINT ( 'NONE', #11134 ) ;
#507 = EDGE_CURVE ( 'NONE', #1441, #8710, #8120, .T. ) ;
#509 = AXIS2_PLACEMENT_3D ( 'NONE', #5543, #4271, #3272 ) ;
#510 = AXIS2_PLACEMENT_3D ( 'NONE', #2408, #4557, #10392 ) ;
#511 = VERTEX_POINT ( 'NONE', #12427 ) ;
#512 = CARTESIAN_POINT ( 'NONE',  ( 49.00442420935993226, -30.80502811811213704, -10.50000000000000000 ) ) ;
#513 = AXIS2_PLACEMENT_3D ( 'NONE', #2469, #8396, #7236 ) ;
#514 = ORIENTED_EDGE ( 'NONE', *, *, #273, .T. ) ;
#515 = EDGE_CURVE ( 'NONE', #15011, #5203, #11902, .T. ) ;
#516 = CYLINDRICAL_SURFACE ( 'NONE', #8350, 0.5000000000000004441 ) ;
#517 = CARTESIAN_POINT ( 'NONE',  ( 4.175648173966053811, -2.207990556236549828, -3.469390959564066623 ) ) ;
#518 =( LENGTH_UNIT ( ) NAMED_UNIT ( * ) SI_UNIT ( .MILLI., .METRE. ) );
#519 = ORIENTED_EDGE ( 'NONE', *, *, #12444, .F. ) ;
#521 = CIRCLE ( 'NONE', #9000, 0.5000000000000073275 ) ;
#520 = CARTESIAN_POINT ( 'NONE',  ( -89.61631465359519666, -37.12029293941281338, -8.000000000000000000 ) ) ;
#522 = LINE ( 'NONE', #1661, #13817 ) ;
#523 = ORIENTED_EDGE ( 'NONE', *, *, #3292, .T. ) ;
#524 = CARTESIAN_POINT ( 'NONE',  ( -12.86891638962156215, 56.43380494353993271, 8.000000000000000000 ) ) ;
#525 = AXIS2_PLACEMENT_3D ( 'NONE', #2311, #1174, #12787 ) ;
#526 = ORIENTED_EDGE ( 'NONE', *, *, #8016, .F. ) ;
#527 = EDGE_LOOP ( 'NONE', ( #759, #3459, #4325, #3794, #1827, #1753, #97, #3731 ) ) ;
#528 = CARTESIAN_POINT ( 'NONE',  ( -32.26435573746199736, 42.04772703543562073, -10.50000000000000000 ) ) ;
#529 =( GEOMETRIC_REPRESENTATION_CONTEXT ( 3 ) GLOBAL_UNCERTAINTY_ASSIGNED_CONTEXT ( ( #3045 ) ) GLOBAL_UNIT_ASSIGNED_CONTEXT ( ( #9128, #5633, #14911 ) ) REPRESENTATION_CONTEXT ( 'NONE', 'WORKASPACE' ) );
#530 = EDGE_CURVE ( 'NONE', #7196, #1593, #12249, .T. ) ;
#531 = CARTESIAN_POINT ( 'NONE',  ( 33.08545438203831424, 101.7020459634810976, -14.77901645503695605 ) ) ;
#532 = EDGE_CURVE ( 'NONE', #4198, #5509, #6823, .T. ) ;
#533 = VECTOR ( 'NONE', #12822, 1000.000000000000000 ) ;
#534 = LINE ( 'NONE', #6277, #10550 ) ;
#535 = DIRECTION ( 'NONE',  ( 0.000000000000000000, 0.000000000000000000, -1.000000000000000000 ) ) ;
#536 = DIRECTION ( 'NONE',  ( 0.000000000000000000, 0.000000000000000000, 1.000000000000000000 ) ) ;
#537 = CARTESIAN_POINT ( 'NONE',  ( -1.144235203016679359, -3.958177651039093359, -0.09382832055446206632 ) ) ;
#538 = ORIENTED_EDGE ( 'NONE', *, *, #13672, .F. ) ;
#539 = EDGE_CURVE ( 'NONE', #11742, #10704, #3490, .T. ) ;
#540 = ORIENTED_EDGE ( 'NONE', *, *, #9437, .T. ) ;
#541 = VECTOR ( 'NONE', #6175, 1000.000000000000114 ) ;
#542 = CARTESIAN_POINT ( 'NONE',  ( 0.000000000000000000, 0.000000000000000000, 8.000000000000000000 ) ) ;
#543 = CARTESIAN_POINT ( 'NONE',  ( 0.000000000000000000, 0.000000000000000000, -23.50000000000000000 ) ) ;
#544 = ORIENTED_EDGE ( 'NONE', *, *, #254, .F. ) ;
#545 = CARTESIAN_POINT ( 'NONE',  ( 52.50000000000000711, -6.429395695523604744E-15, -13.00000000000000178 ) ) ;
#546 = EDGE_CURVE ( 'NONE', #8869, #1076, #7933, .T. ) ;
#547 = DIRECTION ( 'NONE',  ( 0.000000000000000000, 0.000000000000000000, 1.000000000000000000 ) ) ;
#548 = ADVANCED_FACE ( 'NONE', ( #14712 ), #5581, .F. ) ;
#549 = EDGE_LOOP ( 'NONE', ( #11916, #5570, #5078, #10453 ) ) ;
#550 = CARTESIAN_POINT ( 'NONE',  ( 4.204015924366186319, -1.626724848190933104, -3.610627190413391752 ) ) ;
#551 = ORIENTED_EDGE ( 'NONE', *, *, #11963, .T. ) ;
#552 = AXIS2_PLACEMENT_3D ( 'NONE', #4395, #14868, #5594 ) ;
#553 = CIRCLE ( 'NONE', #2254, 53.55662432702593634 ) ;
#554 = DIRECTION ( 'NONE',  ( 0.000000000000000000, 0.000000000000000000, -1.000000000000000000 ) ) ;
#555 = CARTESIAN_POINT ( 'NONE',  ( -99.48933418828642061, 1.674280531760366397, -13.00000000000000178 ) ) ;
#556 = CARTESIAN_POINT ( 'NONE',  ( -10.71740939043329099, 51.19406879332069593, -8.000000000000000000 ) ) ;
#557 = DIRECTION ( 'NONE',  ( 0.000000000000000000, 0.000000000000000000, 1.000000000000000000 ) ) ;
#558 = CARTESIAN_POINT ( 'NONE',  ( -49.54657765281192638, 6.917888187662934563, -13.00000000000000178 ) ) ;
#559 = EDGE_CURVE ( 'NONE', #13798, #2876, #5911, .T. ) ;
#560 = CARTESIAN_POINT ( 'NONE',  ( 0.000000000000000000, 1.178949249685208533, -2.042000000000002036 ) ) ;
#561 = AXIS2_PLACEMENT_3D ( 'NONE', #11375, #4319, #5377 ) ;
#562 = ORIENTED_EDGE ( 'NONE', *, *, #918, .T. ) ;
#563 = DIRECTION ( 'NONE',  ( 1.000000000000000000, 0.000000000000000000, -0.000000000000000000 ) ) ;
#564 = LINE ( 'NONE', #14460, #13714 ) ;
#565 = CIRCLE ( 'NONE', #11245, 3.000000000000002665 ) ;
#566 = CARTESIAN_POINT ( 'NONE',  ( 4.211399257449707889, -2.459727064652520223, -3.751161691472419513 ) ) ;
#567 = UNCERTAINTY_MEASURE_WITH_UNIT (LENGTH_MEASURE( 1.000000000000000082E-05 ), #7702, 'distance_accuracy_value', 'NONE');
#568 = ORIENTED_EDGE ( 'NONE', *, *, #9060, .T. ) ;
#569 = DIRECTION ( 'NONE',  ( -1.000000000000000000, 0.000000000000000000, 0.000000000000000000 ) ) ;
#570 = TOROIDAL_SURFACE ( 'NONE', #4222, 4.000000000000000000, 0.2500000000000000000 ) ;
#571 = VERTEX_POINT ( 'NONE', #13948 ) ;
#572 = CARTESIAN_POINT ( 'NONE',  ( -45.89934640057513349, 26.50000000000019540, -13.00000000000000178 ) ) ;
#573 = CARTESIAN_POINT ( 'NONE',  ( 0.000000000000000000, 0.000000000000000000, 10.50000000000000000 ) ) ;
#574 = AXIS2_PLACEMENT_3D ( 'NONE', #13413, #6560, #8919 ) ;
#575 = DIRECTION ( 'NONE',  ( 1.000000000000000000, 0.000000000000000000, 0.000000000000000000 ) ) ;
#576 = PLANE ( 'NONE',  #9518 ) ;
#577 = CARTESIAN_POINT ( 'NONE',  ( -22.33583958711380646, -30.74264578624812927, -33.00000000000000000 ) ) ;
#578 = CARTESIAN_POINT ( 'NONE',  ( -30.00974697327757212, 96.43868009418278575, -12.76250177908513983 ) ) ;
#579 = ORIENTED_EDGE ( 'NONE', *, *, #13350, .F. ) ;
#580 = ORIENTED_EDGE ( 'NONE', *, *, #4644, .T. ) ;
#581 = AXIS2_PLACEMENT_3D ( 'NONE', #4135, #2990, #8826 ) ;
#582 = CARTESIAN_POINT ( 'NONE',  ( 33.48561063518626923, -47.21331623427104063, -10.50000000000000000 ) ) ;
#583 = CARTESIAN_POINT ( 'NONE',  ( -2.449293598294700991E-16, 97.00000000000000000, -8.000000000000000000 ) ) ;
#584 = CIRCLE ( 'NONE', #9055, 2.649999999999985700 ) ;
#585 = CARTESIAN_POINT ( 'NONE',  ( 92.38795325112850776, -38.26834323650940206, -8.000000000000000000 ) ) ;
#586 = ORIENTED_EDGE ( 'NONE', *, *, #14556, .F. ) ;
#587 = ORIENTED_EDGE ( 'NONE', *, *, #12141, .T. ) ;
#588 = DIRECTION ( 'NONE',  ( 0.000000000000000000, 0.000000000000000000, -1.000000000000000000 ) ) ;
#589 = ORIENTED_EDGE ( 'NONE', *, *, #14748, .F. ) ;
#590 = AXIS2_PLACEMENT_3D ( 'NONE', #2229, #4657, #11799 ) ;
#591 = CIRCLE ( 'NONE', #10537, 57.00000000000000000 ) ;
#592 = CYLINDRICAL_SURFACE ( 'NONE', #2055, 60.50000000000000000 ) ;
#593 = EDGE_CURVE ( 'NONE', #13762, #8214, #2527, .T. ) ;
#594 = AXIS2_PLACEMENT_3D ( 'NONE', #4541, #9080, #9230 ) ;
#595 = EDGE_CURVE ( 'NONE', #13877, #3975, #10764, .T. ) ;
#596 = CARTESIAN_POINT ( 'NONE',  ( -49.00442420935969778, 30.80502811811250297, -8.000000000000000000 ) ) ;
#597 = ADVANCED_FACE ( 'NONE', ( #8308 ), #37, .T. ) ;
#598 = ADVANCED_FACE ( 'NONE', ( #5949 ), #10588, .T. ) ;
#599 = LINE ( 'NONE', #5072, #14330 ) ;
#600 = DIRECTION ( 'NONE',  ( -0.000000000000000000, -0.000000000000000000, -1.000000000000000000 ) ) ;
#601 = EDGE_LOOP ( 'NONE', ( #6163, #9721, #13299, #11953, #1874, #3782 ) ) ;
#602 = EDGE_CURVE ( 'NONE', #14931, #14224, #3501, .T. ) ;
#603 = DIRECTION ( 'NONE',  ( 1.000000000000000000, 0.000000000000000000, 0.000000000000000000 ) ) ;
#604 = VERTEX_POINT ( 'NONE', #4820 ) ;
#605 = CIRCLE ( 'NONE', #4490, 0.5000000000000004441 ) ;
#606 = VECTOR ( 'NONE', #13411, 1000.000000000000000 ) ;
#607 = CIRCLE ( 'NONE', #6899, 50.00000000000000000 ) ;
#608 = VECTOR ( 'NONE', #7160, 1000.000000000000000 ) ;
#609 = ORIENTED_EDGE ( 'NONE', *, *, #9991, .T. ) ;
#610 = EDGE_CURVE ( 'NONE', #5547, #3032, #3461, .T. ) ;
#611 = AXIS2_PLACEMENT_3D ( 'NONE', #784, #938, #10032 ) ;
#612 = ORIENTED_EDGE ( 'NONE', *, *, #6268, .F. ) ;
#613 = CARTESIAN_POINT ( 'NONE',  ( -31.56843276583338209, 95.94012674102927463, 14.97885581718526105 ) ) ;
#614 = CARTESIAN_POINT ( 'NONE',  ( -45.96504489225991819, 23.50071946824089153, -13.00000000000000178 ) ) ;
#615 = AXIS2_PLACEMENT_3D ( 'NONE', #10778, #2654, #11932 ) ;
#616 = DIRECTION ( 'NONE',  ( -1.000000000000000000, 1.749300984178292964E-15, 0.000000000000000000 ) ) ;
#617 = CARTESIAN_POINT ( 'NONE',  ( -39.61975340586619865, -91.27544013909722764, -8.000000000000000000 ) ) ;
#618 = FACE_OUTER_BOUND ( 'NONE', #7850, .T. ) ;
#619 = EDGE_CURVE ( 'NONE', #5663, #6408, #262, .T. ) ;
#620 = AXIS2_PLACEMENT_3D ( 'NONE', #14211, #2814, #7278 ) ;
#621 = FACE_OUTER_BOUND ( 'NONE', #249, .T. ) ;
#622 = ORIENTED_EDGE ( 'NONE', *, *, #8927, .F. ) ;
#623 = CYLINDRICAL_SURFACE ( 'NONE', #7215, 4.999999999999998224 ) ;
#624 = VECTOR ( 'NONE', #11823, 1000.000000000000000 ) ;
#625 = CARTESIAN_POINT ( 'NONE',  ( 2.500000000000002220, 2.357898499370430834, -6.938893903907228378E-15 ) ) ;
#626 = DIRECTION ( 'NONE',  ( 1.000000000000000000, 0.000000000000000000, 0.000000000000000000 ) ) ;
#627 = VECTOR ( 'NONE', #12367, 1000.000000000000000 ) ;
#628 = VERTEX_POINT ( 'NONE', #10436 ) ;
#629 = CARTESIAN_POINT ( 'NONE',  ( 32.78625152019765210, 95.53054288192240051, -15.68243957109766207 ) ) ;
#630 = EDGE_LOOP ( 'NONE', ( #6480, #10245, #8845, #11971, #6286 ) ) ;
#631 = CARTESIAN_POINT ( 'NONE',  ( 3.999999999999996447, 0.3987449864460007043, -0.01220643443059539826 ) ) ;
#632 = ORIENTED_EDGE ( 'NONE', *, *, #5312, .F. ) ;
#633 = CARTESIAN_POINT ( 'NONE',  ( -34.12029293941441210, -89.61631465359452875, -13.00000000000000178 ) ) ;
#634 = ORIENTED_EDGE ( 'NONE', *, *, #8025, .T. ) ;
#635 = CARTESIAN_POINT ( 'NONE',  ( 5.000000000000007994, 0.000000000000000000, 2.775557561562891351E-14 ) ) ;
#636 = DIRECTION ( 'NONE',  ( 1.000000000000000000, 0.000000000000000000, 0.000000000000000000 ) ) ;
#637 = DIRECTION ( 'NONE',  ( 0.000000000000000000, 0.000000000000000000, 1.000000000000000000 ) ) ;
#638 = AXIS2_PLACEMENT_3D ( 'NONE', #14300, #5118, #7308 ) ;
#639 = DIRECTION ( 'NONE',  ( 0.000000000000000000, 0.000000000000000000, 1.000000000000000000 ) ) ;
#640 = CARTESIAN_POINT ( 'NONE',  ( 68.58935777509475429, -68.58935777509547904, -13.00000000000000178 ) ) ;
#641 = CARTESIAN_POINT ( 'NONE',  ( -12.39897948556635754, 94.18739463280904545, 16.00000000000000000 ) ) ;
#642 = EDGE_CURVE ( 'NONE', #4677, #13856, #12948, .T. ) ;
#643 = EDGE_LOOP ( 'NONE', ( #12832, #6192, #9404, #8598 ) ) ;
#644 = ADVANCED_FACE ( 'NONE', ( #9293 ), #3542, .F. ) ;
#645 = LINE ( 'NONE', #13535, #6936 ) ;
#646 = CARTESIAN_POINT ( 'NONE',  ( 25.00000000000000000, 81.24038404635960831, 31.00000000000000000 ) ) ;
#647 = EDGE_CURVE ( 'NONE', #11532, #9553, #13946, .T. ) ;
#648 = CARTESIAN_POINT ( 'NONE',  ( -50.69406879332065330, -13.71740939043347041, 10.49999999999999822 ) ) ;
#649 = AXIS2_PLACEMENT_3D ( 'NONE', #4532, #12650, #12572 ) ;
#650 = ORIENTED_EDGE ( 'NONE', *, *, #11602, .F. ) ;
#651 = EDGE_CURVE ( 'NONE', #7439, #5954, #12735, .T. ) ;
#652 = DIRECTION ( 'NONE',  ( -1.000000000000000000, 0.000000000000000000, 0.000000000000000000 ) ) ;
#653 = ORIENTED_EDGE ( 'NONE', *, *, #14248, .F. ) ;
#654 = CIRCLE ( 'NONE', #3811, 60.50000000000000000 ) ;
#655 = CARTESIAN_POINT ( 'NONE',  ( 0.000000000000000000, 0.000000000000000000, -10.50000000000000000 ) ) ;
#656 = CARTESIAN_POINT ( 'NONE',  ( -56.43380494354004639, -12.86891638962099549, -10.50000000000000000 ) ) ;
#657 = EDGE_LOOP ( 'NONE', ( #3709, #5297, #9603, #4959, #1883 ) ) ;
#658 = CARTESIAN_POINT ( 'NONE',  ( 8.076099607191862262, 62.48290387921808531, -20.00000000000000355 ) ) ;
#659 = CARTESIAN_POINT ( 'NONE',  ( 30.00000000000000355, 97.48846085563152997, 31.00000000000000000 ) ) ;
#660 = DIRECTION ( 'NONE',  ( 1.000000000000000000, 0.000000000000000000, 0.000000000000000000 ) ) ;
#661 = EDGE_LOOP ( 'NONE', ( #9242, #12653, #10598, #12423, #14869 ) ) ;
#662 = CIRCLE ( 'NONE', #12537, 60.50000000000000000 ) ;
#663 = ORIENTED_EDGE ( 'NONE', *, *, #14844, .F. ) ;
#664 = VERTEX_POINT ( 'NONE', #8004 ) ;
#665 = EDGE_CURVE ( 'NONE', #7876, #8214, #5795, .T. ) ;
#666 = CARTESIAN_POINT ( 'NONE',  ( -7.499999999999996447, 85.00000000000000000, 31.00000000000000000 ) ) ;
#667 = CARTESIAN_POINT ( 'NONE',  ( 29.70588235294119173, 96.53269163155674448, 10.99999999999999645 ) ) ;
#668 = DIRECTION ( 'NONE',  ( 0.000000000000000000, 0.000000000000000000, 1.000000000000000000 ) ) ;
#669 = VERTEX_POINT ( 'NONE', #7079 ) ;
#670 = ORIENTED_EDGE ( 'NONE', *, *, #8944, .T. ) ;
#671 = ORIENTED_EDGE ( 'NONE', *, *, #1084, .F. ) ;
#672 = CARTESIAN_POINT ( 'NONE',  ( -12.46631608856921325, 100.2277185551817951, -15.67011936326128563 ) ) ;
#673 = CARTESIAN_POINT ( 'NONE',  ( -19.99999999999998934, 64.99230723708770086, 31.00000000000000000 ) ) ;
#674 = APPLICATION_CONTEXT ( 'automotive_design' ) ;
#675 =( LENGTH_UNIT ( ) NAMED_UNIT ( * ) SI_UNIT ( .MILLI., .METRE. ) );
#676 = CARTESIAN_POINT ( 'NONE',  ( 0.000000000000000000, -1.178949249685208533, 2.042000000000002036 ) ) ;
#677 = CARTESIAN_POINT ( 'NONE',  ( 0.000000000000000000, 0.000000000000000000, -25.50000000000000355 ) ) ;
#678 = CARTESIAN_POINT ( 'NONE',  ( 0.000000000000000000, 0.000000000000000000, -10.50000000000000000 ) ) ;
#679 = ORIENTED_EDGE ( 'NONE', *, *, #5242, .T. ) ;
#680 = DIRECTION ( 'NONE',  ( -1.000000000000000000, 2.312964634635740689E-15, 0.000000000000000000 ) ) ;
#681 = AXIS2_PLACEMENT_3D ( 'NONE', #14508, #12588, #11545 ) ;
#682 = ORIENTED_EDGE ( 'NONE', *, *, #13960, .F. ) ;
#683 = ORIENTED_EDGE ( 'NONE', *, *, #7014, .T. ) ;
#684 = CARTESIAN_POINT ( 'NONE',  ( -33.83210567914650113, 95.16559600367024530, 15.96768719852781615 ) ) ;
#685 = ADVANCED_FACE ( 'NONE', ( #12725 ), #3271, .T. ) ;
#686 = EDGE_CURVE ( 'NONE', #1445, #27, #6861, .T. ) ;
#687 = DIRECTION ( 'NONE',  ( -0.000000000000000000, -0.000000000000000000, -1.000000000000000000 ) ) ;
#688 = CIRCLE ( 'NONE', #3352, 75.00000000000001421 ) ;
#689 = DIRECTION ( 'NONE',  ( -0.000000000000000000, -0.000000000000000000, 1.000000000000000000 ) ) ;
#690 = DIRECTION ( 'NONE',  ( 1.000000000000000000, 0.000000000000000000, 0.000000000000000000 ) ) ;
#691 = CARTESIAN_POINT ( 'NONE',  ( 97.41488903138106537, -0.2790467552935826934, 10.49999999999999822 ) ) ;
#692 = ORIENTED_EDGE ( 'NONE', *, *, #8053, .F. ) ;
#693 = FACE_BOUND ( 'NONE', #8642, .T. ) ;
#694 = EDGE_CURVE ( 'NONE', #12241, #13116, #2321, .T. ) ;
#695 = DIRECTION ( 'NONE',  ( 0.000000000000000000, 0.000000000000000000, 1.000000000000000000 ) ) ;
#696 = CARTESIAN_POINT ( 'NONE',  ( -13.71740939043329277, 51.19406879332069593, -13.00000000000000178 ) ) ;
#697 = VERTEX_POINT ( 'NONE', #5872 ) ;
#698 = CARTESIAN_POINT ( 'NONE',  ( 0.000000000000000000, 0.000000000000000000, 31.00000000000000000 ) ) ;
#699 = EDGE_CURVE ( 'NONE', #5509, #721, #10511, .T. ) ;
#700 = EDGE_CURVE ( 'NONE', #197, #2566, #14081, .T. ) ;
#701 = DIRECTION ( 'NONE',  ( -1.000000000000000000, 0.000000000000000000, 0.000000000000000000 ) ) ;
#702 = ORIENTED_EDGE ( 'NONE', *, *, #1068, .F. ) ;
#703 = DIRECTION ( 'NONE',  ( 0.000000000000000000, 0.000000000000000000, 1.000000000000000000 ) ) ;
#704 = ORIENTED_EDGE ( 'NONE', *, *, #2823, .T. ) ;
#705 = CARTESIAN_POINT ( 'NONE',  ( -11.47921512510733422, 94.30438942219511489, -18.08174836683881992 ) ) ;
#706 = CARTESIAN_POINT ( 'NONE',  ( -68.08935777509570642, -68.58935777509452691, 10.49999999999999822 ) ) ;
#707 = DIRECTION ( 'NONE',  ( 1.000000000000000000, 0.000000000000000000, -0.000000000000000000 ) ) ;
#708 = CARTESIAN_POINT ( 'NONE',  ( 97.00000000000000000, -3.384287605079545030E-13, -13.00000000000000178 ) ) ;
#709 = CARTESIAN_POINT ( 'NONE',  ( -56.43380494354004639, -12.86891638962099549, -10.50000000000000000 ) ) ;
#710 = VECTOR ( 'NONE', #9042, 1000.000000000000000 ) ;
#711 = CARTESIAN_POINT ( 'NONE',  ( 45.96504489226007450, -23.50071946824056823, 8.000000000000000000 ) ) ;
#712 = ORIENTED_EDGE ( 'NONE', *, *, #2162, .T. ) ;
#713 = DIRECTION ( 'NONE',  ( -1.000000000000000000, 0.000000000000000000, 0.000000000000000000 ) ) ;
#714 = DIRECTION ( 'NONE',  ( 0.000000000000000000, 0.000000000000000000, 1.000000000000000000 ) ) ;
#715 = DIRECTION ( 'NONE',  ( 0.000000000000000000, 0.4999999999999995559, -0.8660254037844389297 ) ) ;
#716 = ORIENTED_EDGE ( 'NONE', *, *, #2095, .T. ) ;
#717 = DIRECTION ( 'NONE',  ( -0.000000000000000000, -0.000000000000000000, 1.000000000000000000 ) ) ;
#718 = ADVANCED_FACE ( 'NONE', ( #2614 ), #6307, .T. ) ;
#719 = VECTOR ( 'NONE', #151, 1000.000000000000000 ) ;
#720 = ADVANCED_FACE ( 'NONE', ( #6388 ), #10963, .T. ) ;
#721 = VERTEX_POINT ( 'NONE', #13248 ) ;
#722 = EDGE_CURVE ( 'NONE', #1196, #1453, #2766, .T. ) ;
#723 = DIRECTION ( 'NONE',  ( 0.000000000000000000, 0.000000000000000000, 1.000000000000000000 ) ) ;
#724 = ADVANCED_FACE ( 'NONE', ( #7388 ), #9813, .F. ) ;
#725 = CARTESIAN_POINT ( 'NONE',  ( 11.83526203526748333, 106.3435961965382290, -17.51264358390114140 ) ) ;
#726 = CARTESIAN_POINT ( 'NONE',  ( 34.62083247296202160, 87.95718916809205723, 8.000000000000000000 ) ) ;
#727 =( NAMED_UNIT ( * ) SI_UNIT ( $, .STERADIAN. ) SOLID_ANGLE_UNIT ( ) );
#728 = ORIENTED_EDGE ( 'NONE', *, *, #11280, .F. ) ;
#729 = PRODUCT_DEFINITION_FORMATION_WITH_SPECIFIED_SOURCE ( 'ANY', '', #6312, .NOT_KNOWN. ) ;
#730 = ORIENTED_EDGE ( 'NONE', *, *, #3331, .F. ) ;
#731 = EDGE_LOOP ( 'NONE', ( #3868, #9736, #5381, #217, #12088 ) ) ;
#732 = VECTOR ( 'NONE', #5789, 1000.000000000000000 ) ;
#733 = EDGE_CURVE ( 'NONE', #11315, #4753, #8530, .T. ) ;
#734 = CARTESIAN_POINT ( 'NONE',  ( -96.58511096861892042, -0.2790467552922097916, -13.00000000000000178 ) ) ;
#735 = AXIS2_PLACEMENT_3D ( 'NONE', #8739, #10180, #785 ) ;
#736 = CARTESIAN_POINT ( 'NONE',  ( 35.50766591049263354, 100.5715065882092460, 15.96896126722778497 ) ) ;
#737 = CIRCLE ( 'NONE', #7019, 3.000000000000002665 ) ;
#738 = DIRECTION ( 'NONE',  ( 1.000000000000000000, 0.000000000000000000, 0.000000000000000000 ) ) ;
#739 = EDGE_LOOP ( 'NONE', ( #11744, #3948, #14361, #10298 ) ) ;
#740 = ORIENTED_EDGE ( 'NONE', *, *, #5593, .F. ) ;
#741 = ADVANCED_FACE ( 'NONE', ( #14379 ), #10736, .F. ) ;
#742 = ORIENTED_EDGE ( 'NONE', *, *, #5549, .F. ) ;
#743 = AXIS2_PLACEMENT_3D ( 'NONE', #8201, #3353, #9406 ) ;
#744 = EDGE_CURVE ( 'NONE', #1887, #14718, #1554, .T. ) ;
#745 = AXIS2_PLACEMENT_3D ( 'NONE', #14612, #4209, #7608 ) ;
#746 = CARTESIAN_POINT ( 'NONE',  ( 0.000000000000000000, 0.000000000000000000, -25.03750572909317285 ) ) ;
#747 = VECTOR ( 'NONE', #10628, 1000.000000000000000 ) ;
#748 = AXIS2_PLACEMENT_3D ( 'NONE', #65, #12824, #6815 ) ;
#749 = DIRECTION ( 'NONE',  ( 0.000000000000000000, 0.000000000000000000, 1.000000000000000000 ) ) ;
#750 = SURFACE_SIDE_STYLE ('',( #10079 ) ) ;
#751 = CARTESIAN_POINT ( 'NONE',  ( 42.04772703543530099, 32.26435573746242369, -10.50000000000000000 ) ) ;
#752 = ORIENTED_EDGE ( 'NONE', *, *, #5151, .T. ) ;
#753 = CARTESIAN_POINT ( 'NONE',  ( 50.00000000000000000, -6.123233995736766085E-15, -13.00000000000000178 ) ) ;
#754 = CARTESIAN_POINT ( 'NONE',  ( -31.63177518854774206, 102.2170822241992454, 12.29884221335728789 ) ) ;
#755 = ORIENTED_EDGE ( 'NONE', *, *, #10454, .F. ) ;
#756 = AXIS2_PLACEMENT_3D ( 'NONE', #6672, #13513, #11168 ) ;
#757 = FACE_OUTER_BOUND ( 'NONE', #7860, .T. ) ;
#758 = AXIS2_PLACEMENT_3D ( 'NONE', #11388, #9323, #6891 ) ;
#759 = ORIENTED_EDGE ( 'NONE', *, *, #10762, .F. ) ;
#760 = AXIS2_PLACEMENT_3D ( 'NONE', #9897, #8613, #7466 ) ;
#761 = ORIENTED_EDGE ( 'NONE', *, *, #6262, .F. ) ;
#762 = CARTESIAN_POINT ( 'NONE',  ( -34.44830544488820578, 94.94374256356071839, 16.00000000000000000 ) ) ;
#763 = DIRECTION ( 'NONE',  ( 0.000000000000000000, 0.000000000000000000, -1.000000000000000000 ) ) ;
#764 = AXIS2_PLACEMENT_3D ( 'NONE', #3724, #299, #9545 ) ;
#765 = UNCERTAINTY_MEASURE_WITH_UNIT (LENGTH_MEASURE( 1.000000000000000082E-05 ), #9684, 'distance_accuracy_value', 'NONE');
#766 = CARTESIAN_POINT ( 'NONE',  ( 26.01305530232562546, 46.81487971942612347, -10.50000000000000000 ) ) ;
#767 = LINE ( 'NONE', #13582, #7256 ) ;
#768 = CIRCLE ( 'NONE', #6284, 56.99999999999999289 ) ;
#769 = CARTESIAN_POINT ( 'NONE',  ( 12.86891638962116247, -56.43380494354001087, 10.49999999999999822 ) ) ;
#770 = AXIS2_PLACEMENT_3D ( 'NONE', #14698, #10278, #9977 ) ;
#771 = EDGE_LOOP ( 'NONE', ( #13238, #9884, #2856, #4385 ) ) ;
#772 = DIRECTION ( 'NONE',  ( -1.000000000000000000, 0.000000000000000000, 0.000000000000000000 ) ) ;
#773 = DIRECTION ( 'NONE',  ( 0.000000000000000000, 0.000000000000000000, 1.000000000000000000 ) ) ;
#774 = PLANE ( 'NONE',  #6790 ) ;
#775 = AXIS2_PLACEMENT_3D ( 'NONE', #14759, #8899, #5996 ) ;
#776 = EDGE_LOOP ( 'NONE', ( #8992, #2169, #9336, #8022 ) ) ;
#777 = CARTESIAN_POINT ( 'NONE',  ( 29.86020745210524296, 96.48508785265609333, -12.30285360678859696 ) ) ;
#778 = DIRECTION ( 'NONE',  ( -0.000000000000000000, -0.000000000000000000, -1.000000000000000000 ) ) ;
#779 = AXIS2_PLACEMENT_3D ( 'NONE', #4370, #14539, #5572 ) ;
#780 = ORIENTED_EDGE ( 'NONE', *, *, #9429, .T. ) ;
#781 = DIRECTION ( 'NONE',  ( 0.000000000000000000, 0.000000000000000000, 1.000000000000000000 ) ) ;
#782 = EDGE_LOOP ( 'NONE', ( #5644, #459, #8549, #7892 ) ) ;
#783 = ORIENTED_EDGE ( 'NONE', *, *, #4911, .T. ) ;
#784 = CARTESIAN_POINT ( 'NONE',  ( 0.000000000000000000, 0.000000000000000000, -8.000000000000000000 ) ) ;
#785 = DIRECTION ( 'NONE',  ( 1.000000000000000000, 0.000000000000000000, 0.000000000000000000 ) ) ;
#786 = DIRECTION ( 'NONE',  ( 0.000000000000000000, 0.000000000000000000, 1.000000000000000000 ) ) ;
#787 = CIRCLE ( 'NONE', #2439, 53.55662432702593634 ) ;
#788 = CYLINDRICAL_SURFACE ( 'NONE', #4138, 0.5000000000000038858 ) ;
#789 = ADVANCED_FACE ( 'NONE', ( #417 ), #5271, .F. ) ;
#790 = DIRECTION ( 'NONE',  ( 1.000000000000000000, 0.000000000000000000, 0.000000000000000000 ) ) ;
#791 = ADVANCED_FACE ( 'NONE', ( #3767 ), #10878, .F. ) ;
#792 = EDGE_CURVE ( 'NONE', #9114, #5585, #14918, .T. ) ;
#793 = ORIENTED_EDGE ( 'NONE', *, *, #6481, .F. ) ;
#794 = DIRECTION ( 'NONE',  ( 1.000000000000000000, 0.000000000000000000, 0.000000000000000000 ) ) ;
#795 = ORIENTED_EDGE ( 'NONE', *, *, #10804, .F. ) ;
#796 = STYLED_ITEM ( 'NONE', ( #2153 ), #14006 ) ;
#797 = DIRECTION ( 'NONE',  ( 0.000000000000000000, 0.000000000000000000, 1.000000000000000000 ) ) ;
#798 = DIRECTION ( 'NONE',  ( 1.000000000000000000, 0.000000000000000000, 0.000000000000000000 ) ) ;
#799 = DIRECTION ( 'NONE',  ( 0.000000000000000000, 0.000000000000000000, 1.000000000000000000 ) ) ;
#800 = EDGE_CURVE ( 'NONE', #13568, #2920, #2306, .T. ) ;
#801 = AXIS2_PLACEMENT_3D ( 'NONE', #7638, #12285, #12205 ) ;
#802 = ORIENTED_EDGE ( 'NONE', *, *, #11867, .T. ) ;
#803 = LINE ( 'NONE', #5569, #8515 ) ;
#804 = ORIENTED_EDGE ( 'NONE', *, *, #9181, .F. ) ;
#805 = CIRCLE ( 'NONE', #4679, 0.5000000000000004441 ) ;
#806 = DIRECTION ( 'NONE',  ( -1.000000000000000000, 0.000000000000000000, -0.000000000000000000 ) ) ;
#807 = CARTESIAN_POINT ( 'NONE',  ( -42.04772703543551415, -32.26435573746212526, -13.00000000000000178 ) ) ;
#808 = LINE ( 'NONE', #12276, #11652 ) ;
#809 = CARTESIAN_POINT ( 'NONE',  ( 12.86891638962116247, -56.43380494354001087, -10.50000000000000000 ) ) ;
#810 = SHAPE_DEFINITION_REPRESENTATION ( #4040, #12767 ) ;
#811 = ORIENTED_EDGE ( 'NONE', *, *, #3044, .F. ) ;
#812 = ORIENTED_EDGE ( 'NONE', *, *, #10110, .F. ) ;
#813 = AXIS2_PLACEMENT_3D ( 'NONE', #14533, #3362, #9132 ) ;
#814 = DIRECTION ( 'NONE',  ( 0.000000000000000000, 0.000000000000000000, 1.000000000000000000 ) ) ;
#815 = CARTESIAN_POINT ( 'NONE',  ( 11.47921512510733422, 94.30438942219511489, 18.08174836683881992 ) ) ;
#816 = AXIS2_PLACEMENT_3D ( 'NONE', #13154, #13008, #2599 ) ;
#817 = EDGE_CURVE ( 'NONE', #5666, #5951, #861, .T. ) ;
#818 = CARTESIAN_POINT ( 'NONE',  ( 29.70588235294119173, 96.53269163155674448, -79.80561291909842225 ) ) ;
#819 = ORIENTED_EDGE ( 'NONE', *, *, #273, .F. ) ;
#820 = VECTOR ( 'NONE', #3846, 1000.000000000000000 ) ;
#821 = ORIENTED_EDGE ( 'NONE', *, *, #12506, .T. ) ;
#822 = EDGE_LOOP ( 'NONE', ( #2151, #1128, #4387, #7220 ) ) ;
#823 = CIRCLE ( 'NONE', #9290, 3.000000000000002665 ) ;
#824 = PLANE ( 'NONE',  #113 ) ;
#825 = CARTESIAN_POINT ( 'NONE',  ( 4.121772567811984089, 51.45950017607689375, -13.00000000000000178 ) ) ;
#826 = FACE_OUTER_BOUND ( 'NONE', #6542, .T. ) ;
#827 = ORIENTED_EDGE ( 'NONE', *, *, #1988, .F. ) ;
#828 = AXIS2_PLACEMENT_3D ( 'NONE', #12344, #8988, #11286 ) ;
#829 = EDGE_LOOP ( 'NONE', ( #9264, #5861, #13271, #12662, #11486, #14467, #7990, #3983, #7476 ) ) ;
#830 = FACE_OUTER_BOUND ( 'NONE', #1962, .T. ) ;
#831 = CARTESIAN_POINT ( 'NONE',  ( -34.93100731845028406, 100.8740421756369301, 15.84356320956306341 ) ) ;
#832 = ORIENTED_EDGE ( 'NONE', *, *, #7672, .F. ) ;
#833 = CARTESIAN_POINT ( 'NONE',  ( -30.00000000000000711, 97.48846085563154418, -26.00000000000000000 ) ) ;
#834 = ADVANCED_FACE ( 'NONE', ( #2693 ), #3913, .F. ) ;
#835 = ADVANCED_FACE ( 'NONE', ( #5120 ), #6173, .T. ) ;
#836 = VERTEX_POINT ( 'NONE', #1698 ) ;
#837 = EDGE_LOOP ( 'NONE', ( #2974, #13482 ) ) ;
#838 = AXIS2_PLACEMENT_3D ( 'NONE', #6617, #7914, #11421 ) ;
#839 = DIRECTION ( 'NONE',  ( 1.000000000000000000, 0.000000000000000000, 0.000000000000000000 ) ) ;
#840 = CIRCLE ( 'NONE', #5187, 59.49999999999999289 ) ;
#841 = CIRCLE ( 'NONE', #3261, 3.000000000000002665 ) ;
#842 = AXIS2_PLACEMENT_3D ( 'NONE', #10115, #4783, #2574 ) ;
#843 = FACE_OUTER_BOUND ( 'NONE', #79, .T. ) ;
#844 = EDGE_CURVE ( 'NONE', #2618, #331, #564, .T. ) ;
#845 = DIRECTION ( 'NONE',  ( 0.9557692240748192347, 0.2941176470588224845, 0.000000000000000000 ) ) ;
#846 = CARTESIAN_POINT ( 'NONE',  ( 0.000000000000000000, 0.000000000000000000, -0.2800830152838856835 ) ) ;
#847 = DIRECTION ( 'NONE',  ( 0.000000000000000000, 0.5000000000000012212, 0.8660254037844380415 ) ) ;
#848 = ORIENTED_EDGE ( 'NONE', *, *, #180, .T. ) ;
#849 = VECTOR ( 'NONE', #15018, 1000.000000000000000 ) ;
#850 = AXIS2_PLACEMENT_3D ( 'NONE', #12106, #9589, #11046 ) ;
#851 = CARTESIAN_POINT ( 'NONE',  ( 0.000000000000000000, 0.000000000000000000, -10.50000000000000000 ) ) ;
#852 = CIRCLE ( 'NONE', #12476, 52.50000000000000711 ) ;
#853 = EDGE_CURVE ( 'NONE', #13570, #6495, #9094, .T. ) ;
#854 = CARTESIAN_POINT ( 'NONE',  ( 8.076072847916476505, 62.48290708766281654, 19.99999999999999645 ) ) ;
#855 = FACE_OUTER_BOUND ( 'NONE', #10621, .T. ) ;
#856 = EDGE_LOOP ( 'NONE', ( #12786, #6236, #14465, #13367, #7872, #10379 ) ) ;
#857 = CARTESIAN_POINT ( 'NONE',  ( 31.56843276583338920, 95.94012674102923199, -14.97885581718525572 ) ) ;
#858 = CIRCLE ( 'NONE', #6169, 101.0000000000000284 ) ;
#859 = DIRECTION ( 'NONE',  ( 0.000000000000000000, 0.000000000000000000, -1.000000000000000000 ) ) ;
#860 = ORIENTED_EDGE ( 'NONE', *, *, #12331, .T. ) ;
#861 = CIRCLE ( 'NONE', #14198, 0.5000000000000004441 ) ;
#862 = CYLINDRICAL_SURFACE ( 'NONE', #12376, 3.000000000000002665 ) ;
#863 = AXIS2_PLACEMENT_3D ( 'NONE', #3956, #5244, #8715 ) ;
#864 = ORIENTED_EDGE ( 'NONE', *, *, #408, .F. ) ;
#865 = CARTESIAN_POINT ( 'NONE',  ( -7.500000000000000000, 94.70348462437907244, -20.00000000000000000 ) ) ;
#866 = LINE ( 'NONE', #6604, #1467 ) ;
#867 = FACE_OUTER_BOUND ( 'NONE', #2559, .T. ) ;
#868 = ORIENTED_EDGE ( 'NONE', *, *, #10994, .T. ) ;
#869 = FACE_OUTER_BOUND ( 'NONE', #12218, .T. ) ;
#870 = DIRECTION ( 'NONE',  ( -0.000000000000000000, -0.000000000000000000, 1.000000000000000000 ) ) ;
#871 = CARTESIAN_POINT ( 'NONE',  ( 68.58935777509523746, 68.58935777509499587, 8.000000000000000000 ) ) ;
#872 = AXIS2_PLACEMENT_3D ( 'NONE', #6826, #11629, #4643 ) ;
#873 = ORIENTED_EDGE ( 'NONE', *, *, #14833, .F. ) ;
#874 = DIRECTION ( 'NONE',  ( 1.000000000000000000, 0.000000000000000000, 0.000000000000000000 ) ) ;
#875 = CARTESIAN_POINT ( 'NONE',  ( 36.14014761921570340, 11.74264578624841171, -28.00000000000000000 ) ) ;
#876 = CARTESIAN_POINT ( 'NONE',  ( 3.999999999999998224, -1.677850389430954214, -3.535268758347605456 ) ) ;
#877 = VERTEX_POINT ( 'NONE', #6466 ) ;
#878 = CARTESIAN_POINT ( 'NONE',  ( 25.00000000000000000, 81.24038404635960831, -31.00000000000000000 ) ) ;
#879 = VERTEX_POINT ( 'NONE', #11117 ) ;
#880 = EDGE_CURVE ( 'NONE', #198, #2094, #14679, .T. ) ;
#881 = CIRCLE ( 'NONE', #5239, 10.00000000000000178 ) ;
#882 = CARTESIAN_POINT ( 'NONE',  ( 17.27884612037405887, 39.14960378788569528, -16.00000000000000000 ) ) ;
#883 = EDGE_CURVE ( 'NONE', #12576, #13345, #3048, .T. ) ;
#884 = ORIENTED_EDGE ( 'NONE', *, *, #9126, .F. ) ;
#885 = DIRECTION ( 'NONE',  ( -1.000000000000000000, 0.000000000000000000, 0.000000000000000000 ) ) ;
#886 = PLANE ( 'NONE',  #14118 ) ;
#887 = ORIENTED_EDGE ( 'NONE', *, *, #9762, .F. ) ;
#888 = CARTESIAN_POINT ( 'NONE',  ( 12.24154204929785372, 106.2975094407664471, -16.61985167119453877 ) ) ;
#889 = CARTESIAN_POINT ( 'NONE',  ( 0.2500000000000002220, 0.000000000000000000, 0.000000000000000000 ) ) ;
#890 = SHAPE_DEFINITION_REPRESENTATION ( #8756, #8100 ) ;
#891 = ORIENTED_EDGE ( 'NONE', *, *, #5512, .T. ) ;
#892 = EDGE_CURVE ( 'NONE', #6431, #4070, #4988, .T. ) ;
#893 = ORIENTED_EDGE ( 'NONE', *, *, #1747, .T. ) ;
#894 = ORIENTED_EDGE ( 'NONE', *, *, #507, .T. ) ;
#895 = AXIS2_PLACEMENT_3D ( 'NONE', #10587, #2460, #13023 ) ;
#896 = FACE_OUTER_BOUND ( 'NONE', #1263, .T. ) ;
#897 = CARTESIAN_POINT ( 'NONE',  ( 12.07539369549097863, 94.22990561005788379, 17.09692597381455315 ) ) ;
#898 = PRODUCT_DEFINITION ( 'UNKNOWN', '', #7251, #8798 ) ;
#899 = FACE_OUTER_BOUND ( 'NONE', #14602, .T. ) ;
#900 = VERTEX_POINT ( 'NONE', #11345 ) ;
#901 = ORIENTED_EDGE ( 'NONE', *, *, #9138, .F. ) ;
#902 = EDGE_CURVE ( 'NONE', #13406, #12353, #9331, .T. ) ;
#903 = ORIENTED_EDGE ( 'NONE', *, *, #8788, .T. ) ;
#904 = AXIS2_PLACEMENT_3D ( 'NONE', #239, #2746, #2670 ) ;
#905 = DIRECTION ( 'NONE',  ( 0.000000000000000000, 0.000000000000000000, 1.000000000000000000 ) ) ;
#906 = DIRECTION ( 'NONE',  ( -0.000000000000000000, -0.000000000000000000, -1.000000000000000000 ) ) ;
#907 = FACE_OUTER_BOUND ( 'NONE', #14733, .T. ) ;
#908 =( LENGTH_UNIT ( ) NAMED_UNIT ( * ) SI_UNIT ( .MILLI., .METRE. ) );
#909 = PLANE ( 'NONE',  #14468 ) ;
#910 = PLANE ( 'NONE',  #6070 ) ;
#911 = CARTESIAN_POINT ( 'NONE',  ( -35.50612649840985569, 100.5723974928649085, 15.96895346309148245 ) ) ;
#912 = ORIENTED_EDGE ( 'NONE', *, *, #1117, .F. ) ;
#913 = DIRECTION ( 'NONE',  ( 0.000000000000000000, 0.000000000000000000, 1.000000000000000000 ) ) ;
#914 = VERTEX_POINT ( 'NONE', #6759 ) ;
#915 = VERTEX_POINT ( 'NONE', #9970 ) ;
#916 = CARTESIAN_POINT ( 'NONE',  ( 68.58935777509523746, 68.58935777509499587, 8.000000000000000000 ) ) ;
#917 = CARTESIAN_POINT ( 'NONE',  ( 92.38795325112879198, 38.26834323650871994, -8.000000000000000000 ) ) ;
#918 = EDGE_CURVE ( 'NONE', #11991, #13011, #1582, .T. ) ;
#919 = CARTESIAN_POINT ( 'NONE',  ( 2.500000000000002220, 0.000000000000000000, 0.000000000000000000 ) ) ;
#920 = ADVANCED_FACE ( 'NONE', ( #5564 ), #14693, .F. ) ;
#921 = EDGE_CURVE ( 'NONE', #4010, #3168, #2065, .T. ) ;
#922 = DIRECTION ( 'NONE',  ( 0.000000000000000000, 0.000000000000000000, 1.000000000000000000 ) ) ;
#923 = CARTESIAN_POINT ( 'NONE',  ( -0.5469614295415043959, 4.303013824935313814, -3.535263753545194287 ) ) ;
#924 = DIRECTION ( 'NONE',  ( -1.000000000000000000, 4.440892098500625373E-15, 0.000000000000000000 ) ) ;
#925 = ORIENTED_EDGE ( 'NONE', *, *, #1390, .T. ) ;
#926 = FACE_OUTER_BOUND ( 'NONE', #7857, .T. ) ;
#927 = EDGE_CURVE ( 'NONE', #10678, #6180, #11510, .T. ) ;
#928 = FACE_OUTER_BOUND ( 'NONE', #13623, .T. ) ;
#929 = DIRECTION ( 'NONE',  ( 0.000000000000000000, -1.000000000000000000, 1.471414886128460880E-15 ) ) ;
#930 = ORIENTED_EDGE ( 'NONE', *, *, #9961, .F. ) ;
#931 = CYLINDRICAL_SURFACE ( 'NONE', #8853, 60.50000000000000000 ) ;
#932 = ORIENTED_EDGE ( 'NONE', *, *, #14579, .T. ) ;
#933 = CARTESIAN_POINT ( 'NONE',  ( 30.88253268887308423, 96.16299873708393875, 14.30432816676292163 ) ) ;
#934 = VECTOR ( 'NONE', #3788, 1000.000000000000000 ) ;
#935 = ORIENTED_EDGE ( 'NONE', *, *, #10386, .T. ) ;
#936 = DIRECTION ( 'NONE',  ( 1.000000000000000000, 0.000000000000000000, -0.000000000000000000 ) ) ;
#937 = EDGE_CURVE ( 'NONE', #3633, #12431, #11256, .T. ) ;
#938 = DIRECTION ( 'NONE',  ( 0.000000000000000000, 0.000000000000000000, -1.000000000000000000 ) ) ;
#939 = CARTESIAN_POINT ( 'NONE',  ( -41.59008834022669987, -32.46576781417940794, 10.49999999999999822 ) ) ;
#940 = DIRECTION ( 'NONE',  ( 1.000000000000000000, 0.000000000000000000, 0.000000000000000000 ) ) ;
#941 = DIRECTION ( 'NONE',  ( 0.000000000000000000, 0.000000000000000000, 1.000000000000000000 ) ) ;
#942 = FACE_OUTER_BOUND ( 'NONE', #13951, .T. ) ;
#943 = DIRECTION ( 'NONE',  ( -0.000000000000000000, -0.000000000000000000, 1.000000000000000000 ) ) ;
#944 = VERTEX_POINT ( 'NONE', #2076 ) ;
#945 = DIRECTION ( 'NONE',  ( -1.000000000000000000, 0.000000000000000000, 0.000000000000000000 ) ) ;
#946 = DIRECTION ( 'NONE',  ( 0.000000000000000000, 0.000000000000000000, 1.000000000000000000 ) ) ;
#947 = CARTESIAN_POINT ( 'NONE',  ( 26.49999999999971578, 45.89934640057541060, -13.00000000000000178 ) ) ;
#948 = AXIS2_PLACEMENT_3D ( 'NONE', #8124, #11226, #14645 ) ;
#949 = ORIENTED_EDGE ( 'NONE', *, *, #12444, .T. ) ;
#950 = DIRECTION ( 'NONE',  ( 0.000000000000000000, 0.000000000000000000, -1.000000000000000000 ) ) ;
#951 = ORIENTED_EDGE ( 'NONE', *, *, #10472, .F. ) ;
#952 = DIRECTION ( 'NONE',  ( 1.000000000000000000, 0.000000000000000000, 0.000000000000000000 ) ) ;
#953 = ORIENTED_EDGE ( 'NONE', *, *, #11366, .F. ) ;
#954 = DIRECTION ( 'NONE',  ( -1.000000000000000000, 0.000000000000000000, 0.000000000000000000 ) ) ;
#955 = DIRECTION ( 'NONE',  ( 0.000000000000000000, 0.000000000000000000, -1.000000000000000000 ) ) ;
#956 = CARTESIAN_POINT ( 'NONE',  ( -34.62083247296263266, -87.95718916809180143, -13.00000000000000178 ) ) ;
#957 = LINE ( 'NONE', #5726, #4707 ) ;
#958 = ORIENTED_EDGE ( 'NONE', *, *, #4574, .T. ) ;
#959 = ORIENTED_EDGE ( 'NONE', *, *, #424, .T. ) ;
#960 = ADVANCED_FACE ( 'NONE', ( #11195 ), #9886, .T. ) ;
#961 = DIRECTION ( 'NONE',  ( 0.000000000000000000, 0.000000000000000000, 1.000000000000000000 ) ) ;
#962 = CARTESIAN_POINT ( 'NONE',  ( 12.28362713749409529, 94.20257980066446635, 16.56510878681792320 ) ) ;
#963 = CARTESIAN_POINT ( 'NONE',  ( 5.000000000000004441, 0.000000000000000000, 2.775557561562891351E-14 ) ) ;
#964 = VERTEX_POINT ( 'NONE', #10043 ) ;
#965 = CIRCLE ( 'NONE', #13557, 3.000000000000002665 ) ;
#966 = ORIENTED_EDGE ( 'NONE', *, *, #7536, .T. ) ;
#967 = VERTEX_POINT ( 'NONE', #5423 ) ;
#968 = CARTESIAN_POINT ( 'NONE',  ( -47.21331623427138879, -33.48561063518577896, -8.000000000000000000 ) ) ;
#969 = DIRECTION ( 'NONE',  ( 1.000000000000000000, 1.687538997430237941E-13, 0.000000000000000000 ) ) ;
#970 = CARTESIAN_POINT ( 'NONE',  ( -36.08010649850015028, 100.2464683348682541, -16.00000000000000000 ) ) ;
#971 =( NAMED_UNIT ( * ) SI_UNIT ( $, .STERADIAN. ) SOLID_ANGLE_UNIT ( ) );
#972 = LINE ( 'NONE', #676, #11811 ) ;
#973 = AXIS2_PLACEMENT_3D ( 'NONE', #11244, #6440, #847 ) ;
#974 = CYLINDRICAL_SURFACE ( 'NONE', #6077, 56.99999999999999289 ) ;
#975 = ORIENTED_EDGE ( 'NONE', *, *, #11787, .T. ) ;
#976 = ADVANCED_FACE ( 'NONE', ( #14532 ), #10189, .F. ) ;
#977 = AXIS2_PLACEMENT_3D ( 'NONE', #8876, #11243, #3047 ) ;
#978 = EDGE_CURVE ( 'NONE', #7811, #2618, #11566, .T. ) ;
#979 = EDGE_CURVE ( 'NONE', #4839, #10382, #4953, .T. ) ;
#980 = DIRECTION ( 'NONE',  ( 1.000000000000000000, 0.000000000000000000, 0.000000000000000000 ) ) ;
#981 = DIRECTION ( 'NONE',  ( 0.000000000000000000, 0.000000000000000000, 1.000000000000000000 ) ) ;
#982 = EDGE_LOOP ( 'NONE', ( #3565, #4421, #12085, #3961, #2352 ) ) ;
#983 = AXIS2_PLACEMENT_3D ( 'NONE', #5104, #3827, #13300 ) ;
#984 = ORIENTED_EDGE ( 'NONE', *, *, #8096, .T. ) ;
#985 = DIRECTION ( 'NONE',  ( 0.000000000000000000, 0.000000000000000000, 1.000000000000000000 ) ) ;
#986 = CONICAL_SURFACE ( 'NONE', #14304, 2.059999999999998721, 0.9599310885968738161 ) ;
#987 = AXIS2_PLACEMENT_3D ( 'NONE', #4430, #6526, #9040 ) ;
#988 = COLOUR_RGB ( '', 0.31764706, 0.68627451, 0.89019608) ;
#989 = ORIENTED_EDGE ( 'NONE', *, *, #651, .T. ) ;
#990 = DIRECTION ( 'NONE',  ( -0.000000000000000000, -0.000000000000000000, 1.000000000000000000 ) ) ;
#991 = DIRECTION ( 'NONE',  ( 0.000000000000000000, 0.000000000000000000, 1.000000000000000000 ) ) ;
#992 = DIRECTION ( 'NONE',  ( 1.000000000000000000, 0.000000000000000000, -0.000000000000000000 ) ) ;
#993 = CARTESIAN_POINT ( 'NONE',  ( -2.725741868436042825, 3.045094352034018126, -3.220599429844233086 ) ) ;
#994 = CIRCLE ( 'NONE', #7761, 10.00000000000000355 ) ;
#995 = FACE_OUTER_BOUND ( 'NONE', #3641, .T. ) ;
#996 = ORIENTED_EDGE ( 'NONE', *, *, #8709, .F. ) ;
#997 = DIRECTION ( 'NONE',  ( 0.000000000000000000, 0.000000000000000000, 1.000000000000000000 ) ) ;
#998 = CIRCLE ( 'NONE', #11917, 60.49999999999999289 ) ;
#999 = CARTESIAN_POINT ( 'NONE',  ( -12.94095225512575809, 48.29629131445349088, -8.000000000000000000 ) ) ;
#1000 = DIRECTION ( 'NONE',  ( -1.000000000000000000, 0.000000000000000000, 0.000000000000000000 ) ) ;
#1001 = EDGE_CURVE ( 'NONE', #10819, #13762, #13999, .T. ) ;
#1002 = ORIENTED_EDGE ( 'NONE', *, *, #1299, .F. ) ;
#1003 = FACE_OUTER_BOUND ( 'NONE', #11210, .T. ) ;
#1004 = AXIS2_PLACEMENT_3D ( 'NONE', #11704, #10399, #6901 ) ;
#1005 = ORIENTED_EDGE ( 'NONE', *, *, #546, .T. ) ;
#1006 = AXIS2_PLACEMENT_3D ( 'NONE', #3634, #3567, #8184 ) ;
#1007 = DIRECTION ( 'NONE',  ( 1.000000000000000000, 0.000000000000000000, 0.000000000000000000 ) ) ;
#1008 = EDGE_CURVE ( 'NONE', #12422, #9491, #11751, .T. ) ;
#1009 = LINE ( 'NONE', #6455, #5344 ) ;
#1010 = CIRCLE ( 'NONE', #5121, 3.000000000000002665 ) ;
#1011 = CARTESIAN_POINT ( 'NONE',  ( -31.74999999999995737, 0.000000000000000000, -2.775557561562891351E-14 ) ) ;
#1012 = CARTESIAN_POINT ( 'NONE',  ( -33.48561063518626923, 47.21331623427104063, -10.50000000000000000 ) ) ;
#1013 = CARTESIAN_POINT ( 'NONE',  ( -48.29629131445345536, -12.94095225512591618, -8.000000000000000000 ) ) ;
#1014 = CARTESIAN_POINT ( 'NONE',  ( -68.58935777509427112, 68.58935777509594800, -10.50000000000000000 ) ) ;
#1015 = DIRECTION ( 'NONE',  ( -0.9557692240748186796, -0.2941176470588241498, 0.000000000000000000 ) ) ;
#1016 = DIRECTION ( 'NONE',  ( 1.000000000000000000, 0.000000000000000000, 0.000000000000000000 ) ) ;
#1017 = AXIS2_PLACEMENT_3D ( 'NONE', #9379, #8526, #13310 ) ;
#1018 = ORIENTED_EDGE ( 'NONE', *, *, #9654, .T. ) ;
#1019 = DIRECTION ( 'NONE',  ( 0.000000000000000000, 0.000000000000000000, 1.000000000000000000 ) ) ;
#1020 = DIRECTION ( 'NONE',  ( -0.000000000000000000, -0.000000000000000000, -1.000000000000000000 ) ) ;
#1021 = ADVANCED_FACE ( 'NONE', ( #10349 ), #5198, .F. ) ;
#1022 = EDGE_CURVE ( 'NONE', #664, #4760, #1315, .T. ) ;
#1023 = CIRCLE ( 'NONE', #7051, 4.000000000000000000 ) ;
#1024 = DIRECTION ( 'NONE',  ( 1.000000000000000000, 0.000000000000000000, 0.000000000000000000 ) ) ;
#1025 = ORIENTED_EDGE ( 'NONE', *, *, #14569, .T. ) ;
#1026 = PRODUCT_DEFINITION_SHAPE ( 'NONE', 'NONE',  #3579 ) ;
#1027 = CARTESIAN_POINT ( 'NONE',  ( -3.999999999999996447, 2.309401076758498039, -5.000000000000000888 ) ) ;
#1028 = ORIENTED_EDGE ( 'NONE', *, *, #2126, .T. ) ;
#1029 = DIRECTION ( 'NONE',  ( -1.000000000000000000, 0.000000000000000000, 0.000000000000000000 ) ) ;
#1030 = EDGE_LOOP ( 'NONE', ( #7241, #8999, #5615, #1735 ) ) ;
#1031 = CIRCLE ( 'NONE', #2237, 56.99999999999999289 ) ;
#1032 = DIRECTION ( 'NONE',  ( 1.000000000000000000, 0.000000000000000000, 0.000000000000000000 ) ) ;
#1033 = DIRECTION ( 'NONE',  ( 1.000000000000000000, 0.000000000000000000, 0.000000000000000000 ) ) ;
#1034 = EDGE_CURVE ( 'NONE', #511, #2333, #1078, .T. ) ;
#1035 = CARTESIAN_POINT ( 'NONE',  ( 7.830013896347493230, 106.7136370351866077, -20.00000000000000355 ) ) ;
#1036 = AXIS2_PLACEMENT_3D ( 'NONE', #8185, #4073, #7031 ) ;
#1037 = CARTESIAN_POINT ( 'NONE',  ( -36.62029293941440500, -89.61631465359452875, 10.49999999999999822 ) ) ;
#1038 = ORIENTED_EDGE ( 'NONE', *, *, #14260, .F. ) ;
#1039 = ORIENTED_EDGE ( 'NONE', *, *, #344, .F. ) ;
#1040 = ORIENTED_EDGE ( 'NONE', *, *, #14569, .F. ) ;
#1041 = ORIENTED_EDGE ( 'NONE', *, *, #6655, .T. ) ;
#1042 = CARTESIAN_POINT ( 'NONE',  ( -11.10302805179279240, 62.01554028455485224, -18.51404809149991237 ) ) ;
#1043 = DIRECTION ( 'NONE',  ( 1.000000000000000000, 0.000000000000000000, 0.000000000000000000 ) ) ;
#1044 = DIRECTION ( 'NONE',  ( 1.000000000000000000, 0.000000000000000000, 0.000000000000000000 ) ) ;
#1045 = ORIENTED_EDGE ( 'NONE', *, *, #3414, .F. ) ;
#1046 = AXIS2_PLACEMENT_3D ( 'NONE', #3307, #13941, #11731 ) ;
#1047 = ORIENTED_EDGE ( 'NONE', *, *, #10839, .F. ) ;
#1048 = ORIENTED_EDGE ( 'NONE', *, *, #4644, .F. ) ;
#1049 = CARTESIAN_POINT ( 'NONE',  ( 7.787661217455939422, 74.59514674284385194, 20.00000000000000000 ) ) ;
#1050 = ADVANCED_FACE ( 'NONE', ( #5639 ), #8067, .T. ) ;
#1051 = VECTOR ( 'NONE', #10496, 1000.000000000000000 ) ;
#1052 = LINE ( 'NONE', #5668, #11439 ) ;
#1053 = CARTESIAN_POINT ( 'NONE',  ( 3.453038570459486589, 2.625189405339789062, -3.535263753543648413 ) ) ;
#1054 = DIRECTION ( 'NONE',  ( 1.000000000000000000, 0.000000000000000000, 0.000000000000000000 ) ) ;
#1055 = VERTEX_POINT ( 'NONE', #12627 ) ;
#1056 = CARTESIAN_POINT ( 'NONE',  ( -37.02125851216292318, 90.10640870805768543, 10.49999999999999822 ) ) ;
#1057 = VECTOR ( 'NONE', #14220, 1000.000000000000114 ) ;
#1058 = ORIENTED_EDGE ( 'NONE', *, *, #12704, .T. ) ;
#1059 = CARTESIAN_POINT ( 'NONE',  ( 31.05588327715837238, -44.79355920668822222, -8.000000000000000000 ) ) ;
#1060 = DIRECTION ( 'NONE',  ( 1.000000000000000000, 0.000000000000000000, 0.000000000000000000 ) ) ;
#1061 = CIRCLE ( 'NONE', #7341, 0.5000000000000004441 ) ;
#1062 = ORIENTED_EDGE ( 'NONE', *, *, #5722, .T. ) ;
#1063 = VECTOR ( 'NONE', #7099, 1000.000000000000000 ) ;
#1064 = ORIENTED_EDGE ( 'NONE', *, *, #4462, .F. ) ;
#1065 = CARTESIAN_POINT ( 'NONE',  ( -4.024497503033713564, 2.323544716729485593, -3.572167766733750582 ) ) ;
#1066 = EDGE_CURVE ( 'NONE', #6492, #1186, #13431, .T. ) ;
#1067 = EDGE_CURVE ( 'NONE', #4053, #6451, #6872, .T. ) ;
#1068 = EDGE_CURVE ( 'NONE', #3184, #14306, #10255, .T. ) ;
#1069 = CARTESIAN_POINT ( 'NONE',  ( -56.43380494354004639, -12.86891638962099549, -13.00000000000000178 ) ) ;
#1070 = DIRECTION ( 'NONE',  ( 0.000000000000000000, 0.000000000000000000, 1.000000000000000000 ) ) ;
#1071 = CIRCLE ( 'NONE', #9763, 63.00000000000000000 ) ;
#1072 = DIRECTION ( 'NONE',  ( 1.000000000000000000, 0.000000000000000000, -0.000000000000000000 ) ) ;
#1073 = DIRECTION ( 'NONE',  ( 0.000000000000000000, 0.000000000000000000, 1.000000000000000000 ) ) ;
#1074 = EDGE_CURVE ( 'NONE', #11288, #23, #6852, .T. ) ;
#1075 = CARTESIAN_POINT ( 'NONE',  ( 0.000000000000000000, 0.000000000000000000, -4.000000000000000000 ) ) ;
#1076 = VERTEX_POINT ( 'NONE', #6921 ) ;
#1077 = LINE ( 'NONE', #9109, #4160 ) ;
#1078 = CIRCLE ( 'NONE', #590, 0.5000000000000073275 ) ;
#1079 = VECTOR ( 'NONE', #8441, 1000.000000000000000 ) ;
#1080 = CARTESIAN_POINT ( 'NONE',  ( 1.836970198721029747E-14, -100.0000000000000000, 8.000000000000000000 ) ) ;
#1081 = DIRECTION ( 'NONE',  ( 0.000000000000000000, -0.5000000000000008882, -0.8660254037844380415 ) ) ;
#1082 = AXIS2_PLACEMENT_3D ( 'NONE', #12825, #7037, #8342 ) ;
#1083 = ORIENTED_EDGE ( 'NONE', *, *, #12114, .T. ) ;
#1084 = EDGE_CURVE ( 'NONE', #7921, #9052, #5933, .T. ) ;
#1085 = DIRECTION ( 'NONE',  ( 1.000000000000000000, 0.000000000000000000, 0.000000000000000000 ) ) ;
#1086 = ORIENTED_EDGE ( 'NONE', *, *, #7949, .F. ) ;
#1087 = DIRECTION ( 'NONE',  ( -1.000000000000000000, -6.217248937900876626E-15, 0.000000000000000000 ) ) ;
#1088 = EDGE_CURVE ( 'NONE', #2988, #1331, #9981, .T. ) ;
#1089 = CARTESIAN_POINT ( 'NONE',  ( -6.451868917687557214, -52.36539807335606156, -13.00000000000000178 ) ) ;
#1090 = DIRECTION ( 'NONE',  ( 0.000000000000000000, 0.000000000000000000, 1.000000000000000000 ) ) ;
#1091 = CARTESIAN_POINT ( 'NONE',  ( -12.33783400350010595, 106.2863213744706172, 16.30550365830425363 ) ) ;
#1092 = DIRECTION ( 'NONE',  ( 1.000000000000000000, 0.000000000000000000, 0.000000000000000000 ) ) ;
#1093 = CIRCLE ( 'NONE', #14668, 3.000000000000002665 ) ;
#1094 = VECTOR ( 'NONE', #12798, 1000.000000000000000 ) ;
#1095 = CIRCLE ( 'NONE', #12238, 3.000000000000002665 ) ;
#1096 = CARTESIAN_POINT ( 'NONE',  ( -3.999999999999998224, -2.472261339043344108, -3.687027428081193214 ) ) ;
#1097 = CARTESIAN_POINT ( 'NONE',  ( 69.08004447556065486, 68.68541276968852571, 10.49999999999999822 ) ) ;
#1098 = ORIENTED_EDGE ( 'NONE', *, *, #13042, .T. ) ;
#1099 = CARTESIAN_POINT ( 'NONE',  ( 7.500000000000000888, 106.2673515243510991, -20.00000000000000000 ) ) ;
#1100 = CARTESIAN_POINT ( 'NONE',  ( -42.04772703543551415, -32.26435573746212526, 10.49999999999999822 ) ) ;
#1101 = DIRECTION ( 'NONE',  ( 0.000000000000000000, 0.000000000000000000, -1.000000000000000000 ) ) ;
#1102 = AXIS2_PLACEMENT_3D ( 'NONE', #1355, #1573, #7176 ) ;
#1103 = VECTOR ( 'NONE', #3208, 1000.000000000000000 ) ;
#1104 = DIRECTION ( 'NONE',  ( -1.000000000000000000, 0.000000000000000000, 0.000000000000000000 ) ) ;
#1105 = ORIENTED_EDGE ( 'NONE', *, *, #8346, .F. ) ;
#1106 = CARTESIAN_POINT ( 'NONE',  ( 12.86891638962116247, -56.43380494354001087, 10.49999999999999822 ) ) ;
#1107 = VERTEX_POINT ( 'NONE', #11720 ) ;
#1108 = DIRECTION ( 'NONE',  ( 0.000000000000000000, 0.000000000000000000, 1.000000000000000000 ) ) ;
#1109 = CARTESIAN_POINT ( 'NONE',  ( 26.99988008862626643, 45.88839665196127271, -10.50000000000000000 ) ) ;
#1110 = EDGE_CURVE ( 'NONE', #4909, #8032, #8144, .T. ) ;
#1111 = CONICAL_SURFACE ( 'NONE', #3536, 4.000000000000000000, 0.8911886515913786111 ) ;
#1112 = FACE_OUTER_BOUND ( 'NONE', #4539, .T. ) ;
#1113 = EDGE_CURVE ( 'NONE', #10850, #5953, #3446, .T. ) ;
#1114 = DIRECTION ( 'NONE',  ( -0.000000000000000000, -0.000000000000000000, 1.000000000000000000 ) ) ;
#1115 = VERTEX_POINT ( 'NONE', #10494 ) ;
#1116 = AXIS2_PLACEMENT_3D ( 'NONE', #9933, #12534, #1823 ) ;
#1117 = EDGE_CURVE ( 'NONE', #7158, #3032, #9540, .T. ) ;
#1118 = ORIENTED_EDGE ( 'NONE', *, *, #13189, .T. ) ;
#1119 = ORIENTED_EDGE ( 'NONE', *, *, #10981, .F. ) ;
#1120 = DIRECTION ( 'NONE',  ( -1.000000000000000000, 0.000000000000000000, 0.000000000000000000 ) ) ;
#1121 = DIRECTION ( 'NONE',  ( 0.000000000000000000, 0.000000000000000000, 1.000000000000000000 ) ) ;
#1122 = DIRECTION ( 'NONE',  ( -1.000000000000000000, 0.000000000000000000, 0.000000000000000000 ) ) ;
#1123 = CIRCLE ( 'NONE', #2560, 0.5000000000000043299 ) ;
#1124 = VERTEX_POINT ( 'NONE', #14065 ) ;
#1125 = EDGE_CURVE ( 'NONE', #13289, #1809, #11865, .T. ) ;
#1126 = AXIS2_PLACEMENT_3D ( 'NONE', #7045, #5916, #10624 ) ;
#1127 = EDGE_LOOP ( 'NONE', ( #6521, #13064, #2206, #269, #930 ) ) ;
#1128 = ORIENTED_EDGE ( 'NONE', *, *, #13331, .F. ) ;
#1129 = CARTESIAN_POINT ( 'NONE',  ( 11.45967689402250755, 74.11957758926655515, 18.06636219913714214 ) ) ;
#1130 = CARTESIAN_POINT ( 'NONE',  ( 52.50000000000000711, -6.429395695523604744E-15, -10.50000000000000000 ) ) ;
#1131 = EDGE_CURVE ( 'NONE', #11551, #469, #6076, .T. ) ;
#1132 = DIRECTION ( 'NONE',  ( -1.000000000000000000, 0.000000000000000000, 0.000000000000000000 ) ) ;
#1133 =( NAMED_UNIT ( * ) SI_UNIT ( $, .STERADIAN. ) SOLID_ANGLE_UNIT ( ) );
#1134 = CARTESIAN_POINT ( 'NONE',  ( 89.89283556784508278, -37.53686968382275779, 10.49999999999999822 ) ) ;
#1135 = ORIENTED_EDGE ( 'NONE', *, *, #927, .F. ) ;
#1136 = DIRECTION ( 'NONE',  ( 1.000000000000000000, 0.000000000000000000, -0.000000000000000000 ) ) ;
#1137 = ORIENTED_EDGE ( 'NONE', *, *, #10454, .T. ) ;
#1138 = ORIENTED_EDGE ( 'NONE', *, *, #13360, .F. ) ;
#1139 = DIRECTION ( 'NONE',  ( -1.000000000000000000, 0.000000000000000000, 0.000000000000000000 ) ) ;
#1140 = CARTESIAN_POINT ( 'NONE',  ( -44.89637028918153305, 0.000000000000000000, 14.49999999999999822 ) ) ;
#1141 = ORIENTED_EDGE ( 'NONE', *, *, #1629, .T. ) ;
#1142 = ORIENTED_EDGE ( 'NONE', *, *, #14457, .F. ) ;
#1143 = CARTESIAN_POINT ( 'NONE',  ( -52.36539807335606156, 6.451868917687758831, -13.00000000000000178 ) ) ;
#1144 = VERTEX_POINT ( 'NONE', #10863 ) ;
#1145 = CARTESIAN_POINT ( 'NONE',  ( -38.79014761921587962, 11.74264578624790190, -25.50000000000000355 ) ) ;
#1146 = DIRECTION ( 'NONE',  ( 1.000000000000000000, 0.000000000000000000, 0.000000000000000000 ) ) ;
#1147 = CARTESIAN_POINT ( 'NONE',  ( -2.500000000000000888, 0.000000000000000000, -4.974599999999998801 ) ) ;
#1148 = CARTESIAN_POINT ( 'NONE',  ( 37.53686968382241673, 89.89283556784525331, 10.49999999999999822 ) ) ;
#1149 = ORIENTED_EDGE ( 'NONE', *, *, #602, .F. ) ;
#1150 = DIRECTION ( 'NONE',  ( 0.000000000000000000, 0.000000000000000000, -1.000000000000000000 ) ) ;
#1151 = ORIENTED_EDGE ( 'NONE', *, *, #5739, .F. ) ;
#1152 = ADVANCED_FACE ( 'NONE', ( #1615 ), #7441, .F. ) ;
#1153 = DIRECTION ( 'NONE',  ( -0.000000000000000000, -0.000000000000000000, 1.000000000000000000 ) ) ;
#1154 = EDGE_CURVE ( 'NONE', #3918, #406, #14383, .T. ) ;
#1155 = VERTEX_POINT ( 'NONE', #13077 ) ;
#1156 = DIRECTION ( 'NONE',  ( 1.000000000000000000, 9.329605248950895679E-16, 0.000000000000000000 ) ) ;
#1157 = FACE_OUTER_BOUND ( 'NONE', #14377, .T. ) ;
#1158 = VERTEX_POINT ( 'NONE', #8439 ) ;
#1159 = DIRECTION ( 'NONE',  ( -1.000000000000000000, 0.000000000000000000, 0.000000000000000000 ) ) ;
#1160 = CARTESIAN_POINT ( 'NONE',  ( 2.500000000000002220, 2.357898499370430834, -6.938893903907228378E-15 ) ) ;
#1161 = DIRECTION ( 'NONE',  ( -1.000000000000000000, 0.000000000000000000, 0.000000000000000000 ) ) ;
#1162 = DIRECTION ( 'NONE',  ( 0.000000000000000000, -1.000000000000000000, 0.000000000000000000 ) ) ;
#1163 = CARTESIAN_POINT ( 'NONE',  ( 49.00442420935993226, -30.80502811811213704, -13.00000000000000178 ) ) ;
#1164 = EDGE_CURVE ( 'NONE', #13227, #8073, #318, .T. ) ;
#1165 = DIRECTION ( 'NONE',  ( 0.000000000000000000, 0.000000000000000000, -1.000000000000000000 ) ) ;
#1166 = ORIENTED_EDGE ( 'NONE', *, *, #6232, .T. ) ;
#1167 = EDGE_CURVE ( 'NONE', #11760, #6451, #6288, .T. ) ;
#1168 = ADVANCED_FACE ( 'NONE', ( #2889 ), #14440, .F. ) ;
#1169 = CARTESIAN_POINT ( 'NONE',  ( 0.000000000000000000, 4.618802153517009401, 0.000000000000000000 ) ) ;
#1170 = DIRECTION ( 'NONE',  ( 1.000000000000000000, 0.000000000000000000, 0.000000000000000000 ) ) ;
#1171 = PLANE ( 'NONE',  #14865 ) ;
#1172 = DIRECTION ( 'NONE',  ( 1.000000000000000000, 0.000000000000000000, 0.000000000000000000 ) ) ;
#1173 = ORIENTED_EDGE ( 'NONE', *, *, #11745, .T. ) ;
#1174 = DIRECTION ( 'NONE',  ( -0.000000000000000000, -0.000000000000000000, 1.000000000000000000 ) ) ;
#1175 = EDGE_LOOP ( 'NONE', ( #12279, #493, #10132, #8231 ) ) ;
#1176 = DIRECTION ( 'NONE',  ( 1.000000000000000000, 0.000000000000000000, 0.000000000000000000 ) ) ;
#1177 = CARTESIAN_POINT ( 'NONE',  ( -3.999999999999997335, 1.563622288139196126, -0.2253451193528282215 ) ) ;
#1178 = CARTESIAN_POINT ( 'NONE',  ( 0.2790467552932288098, 97.41488903138106537, -10.50000000000000000 ) ) ;
#1179 = CARTESIAN_POINT ( 'NONE',  ( 30.80502811811196295, 49.00442420936003174, 10.49999999999999822 ) ) ;
#1180 = ORIENTED_EDGE ( 'NONE', *, *, #14238, .T. ) ;
#1181 = DIRECTION ( 'NONE',  ( 1.000000000000000000, 0.000000000000000000, 0.000000000000000000 ) ) ;
#1182 = CARTESIAN_POINT ( 'NONE',  ( -27.94117647058823550, 90.79807628710781842, 13.50000000000000533 ) ) ;
#1183 = FACE_OUTER_BOUND ( 'NONE', #2396, .T. ) ;
#1184 = ORIENTED_EDGE ( 'NONE', *, *, #9617, .F. ) ;
#1185 = ADVANCED_FACE ( 'NONE', ( #5031 ), #10720, .T. ) ;
#1186 = VERTEX_POINT ( 'NONE', #6155 ) ;
#1187 = ORIENTED_EDGE ( 'NONE', *, *, #10479, .T. ) ;
#1188 = EDGE_CURVE ( 'NONE', #132, #5666, #11485, .T. ) ;
#1189 = DIRECTION ( 'NONE',  ( -1.000000000000000000, 0.000000000000000000, 0.000000000000000000 ) ) ;
#1190 = PLANE ( 'NONE',  #2216 ) ;
#1191 = DIRECTION ( 'NONE',  ( 1.000000000000000000, 0.000000000000000000, 0.000000000000000000 ) ) ;
#1192 = DIRECTION ( 'NONE',  ( -1.000000000000000000, 0.000000000000000000, 0.000000000000000000 ) ) ;
#1193 = ADVANCED_FACE ( 'NONE', ( #8656 ), #240, .F. ) ;
#1194 = DIRECTION ( 'NONE',  ( -1.000000000000000000, 0.000000000000000000, 0.000000000000000000 ) ) ;
#1195 = EDGE_LOOP ( 'NONE', ( #10370, #3333, #13617, #10087, #10514, #11394 ) ) ;
#1196 = VERTEX_POINT ( 'NONE', #5098 ) ;
#1197 = EDGE_LOOP ( 'NONE', ( #4372, #1544, #6897, #8188 ) ) ;
#1198 = CARTESIAN_POINT ( 'NONE',  ( 1.674280531759317014, -94.51066581171355097, 8.000000000000000000 ) ) ;
#1199 = CIRCLE ( 'NONE', #14053, 5.384454397937118664 ) ;
#1200 = DIRECTION ( 'NONE',  ( 0.000000000000000000, 0.000000000000000000, 1.000000000000000000 ) ) ;
#1201 = ORIENTED_EDGE ( 'NONE', *, *, #6664, .F. ) ;
#1202 = ADVANCED_FACE ( 'NONE', ( #14284 ), #398, .T. ) ;
#1203 = ADVANCED_FACE ( 'NONE', ( #1394 ), #3893, .F. ) ;
#1204 = ORIENTED_EDGE ( 'NONE', *, *, #10110, .T. ) ;
#1205 = DIRECTION ( 'NONE',  ( 0.000000000000000000, 0.000000000000000000, 1.000000000000000000 ) ) ;
#1206 = ORIENTED_EDGE ( 'NONE', *, *, #2111, .T. ) ;
#1207 = VERTEX_POINT ( 'NONE', #8367 ) ;
#1208 = PLANE ( 'NONE',  #14822 ) ;
#1209 = AXIS2_PLACEMENT_3D ( 'NONE', #2497, #13132, #377 ) ;
#1210 = CARTESIAN_POINT ( 'NONE',  ( -10.71740939043329099, 51.19406879332069593, -13.00000000000000178 ) ) ;
#1211 = DIRECTION ( 'NONE',  ( -0.000000000000000000, -0.000000000000000000, 1.000000000000000000 ) ) ;
#1212 = CARTESIAN_POINT ( 'NONE',  ( -4.236525694536555697, 2.416953475386462546, -3.751298745799836798 ) ) ;
#1213 = CARTESIAN_POINT ( 'NONE',  ( 0.5000000000000045519, -97.00000000000000000, -10.50000000000000000 ) ) ;
#1214 = EDGE_LOOP ( 'NONE', ( #2822, #10967, #11441, #6951, #1083, #5063, #11913, #14182, #10277, #10821 ) ) ;
#1215 = LINE ( 'NONE', #5836, #7523 ) ;
#1216 = CIRCLE ( 'NONE', #6280, 3.000000000000002665 ) ;
#1217 = AXIS2_PLACEMENT_3D ( 'NONE', #2379, #11733, #5945 ) ;
#1218 = DIRECTION ( 'NONE',  ( 0.000000000000000000, 0.000000000000000000, 1.000000000000000000 ) ) ;
#1219 = ORIENTED_EDGE ( 'NONE', *, *, #11069, .T. ) ;
#1220 = DIRECTION ( 'NONE',  ( -0.000000000000000000, -0.000000000000000000, -1.000000000000000000 ) ) ;
#1221 = ORIENTED_EDGE ( 'NONE', *, *, #12597, .F. ) ;
#1222 = CARTESIAN_POINT ( 'NONE',  ( 0.000000000000000000, 0.000000000000000000, -10.50000000000000000 ) ) ;
#1223 = DIRECTION ( 'NONE',  ( 0.000000000000000000, 0.000000000000000000, 1.000000000000000000 ) ) ;
#1224 = CIRCLE ( 'NONE', #3896, 2.649999999999992806 ) ;
#1225 = CYLINDRICAL_SURFACE ( 'NONE', #2799, 75.00000000000001421 ) ;
#1226 = CARTESIAN_POINT ( 'NONE',  ( -9.104688129943026453, 106.6120509519916766, 19.73833377876426809 ) ) ;
#1227 = CARTESIAN_POINT ( 'NONE',  ( -25.00000000000000000, 81.24038404635962252, 13.50000000000000533 ) ) ;
#1228 = CIRCLE ( 'NONE', #6295, 52.50000000000000711 ) ;
#1229 = FACE_OUTER_BOUND ( 'NONE', #8581, .T. ) ;
#1230 = CONTEXT_DEPENDENT_SHAPE_REPRESENTATION ( #11154, #1857 ) ;
#1231 = CIRCLE ( 'NONE', #1719, 95.00000000000001421 ) ;
#1232 = SHAPE_REPRESENTATION ( 'wheel hub', ( #5108 ), #3871 ) ;
#1233 = DIRECTION ( 'NONE',  ( -1.000000000000000000, 0.000000000000000000, 0.000000000000000000 ) ) ;
#1234 = ORIENTED_EDGE ( 'NONE', *, *, #1022, .T. ) ;
#1235 = VECTOR ( 'NONE', #13228, 1000.000000000000000 ) ;
#1236 = DIRECTION ( 'NONE',  ( 0.000000000000000000, 0.000000000000000000, 1.000000000000000000 ) ) ;
#1237 = DIRECTION ( 'NONE',  ( -0.000000000000000000, -0.000000000000000000, -1.000000000000000000 ) ) ;
#1238 = CARTESIAN_POINT ( 'NONE',  ( 42.50536573064410106, 32.06294366074510549, -13.00000000000000178 ) ) ;
#1239 = AXIS2_PLACEMENT_3D ( 'NONE', #1714, #10749, #12053 ) ;
#1240 = DIRECTION ( 'NONE',  ( -1.000000000000000000, 0.000000000000000000, 0.000000000000000000 ) ) ;
#1241 = VECTOR ( 'NONE', #9615, 1000.000000000000000 ) ;
#1242 = ORIENTED_EDGE ( 'NONE', *, *, #5414, .T. ) ;
#1243 = EDGE_CURVE ( 'NONE', #10452, #4454, #7337, .T. ) ;
#1244 = CARTESIAN_POINT ( 'NONE',  ( -52.54657765281192638, 6.917888187662934563, 8.000000000000000000 ) ) ;
#1245 = ORIENTED_EDGE ( 'NONE', *, *, #1497, .T. ) ;
#1246 = EDGE_CURVE ( 'NONE', #5385, #6488, #9711, .T. ) ;
#1247 = DIRECTION ( 'NONE',  ( -0.000000000000000000, -0.000000000000000000, 1.000000000000000000 ) ) ;
#1248 = EDGE_CURVE ( 'NONE', #7084, #6551, #10502, .T. ) ;
#1249 = DIRECTION ( 'NONE',  ( 0.000000000000000000, 0.000000000000000000, -1.000000000000000000 ) ) ;
#1250 = EDGE_CURVE ( 'NONE', #14881, #9830, #12087, .T. ) ;
#1251 = AXIS2_PLACEMENT_3D ( 'NONE', #2176, #4398, #4475 ) ;
#1252 = CARTESIAN_POINT ( 'NONE',  ( 2.000000000000008882, 3.464101615137750390, 0.000000000000000000 ) ) ;
#1253 = DIRECTION ( 'NONE',  ( 1.000000000000000000, 0.000000000000000000, 0.000000000000000000 ) ) ;
#1254 = ADVANCED_FACE ( 'NONE', ( #3967 ), #1900, .F. ) ;
#1255 = VECTOR ( 'NONE', #2315, 1000.000000000000000 ) ;
#1256 = ORIENTED_EDGE ( 'NONE', *, *, #12226, .T. ) ;
#1257 = AXIS2_PLACEMENT_3D ( 'NONE', #247, #8215, #8072 ) ;
#1258 = CARTESIAN_POINT ( 'NONE',  ( -97.00000000000000000, 1.015776140243522349E-12, 8.000000000000000000 ) ) ;
#1259 = CARTESIAN_POINT ( 'NONE',  ( 2.500000000000002220, 2.357898499370430834, -6.938893903907228378E-15 ) ) ;
#1260 = CARTESIAN_POINT ( 'NONE',  ( 38.26834323650840020, -92.38795325112891987, -8.000000000000000000 ) ) ;
#1261 = ORIENTED_EDGE ( 'NONE', *, *, #13537, .T. ) ;
#1262 = AXIS2_PLACEMENT_3D ( 'NONE', #11581, #9413, #13926 ) ;
#1263 = EDGE_LOOP ( 'NONE', ( #1616, #783, #4201, #4811 ) ) ;
#1264 = VERTEX_POINT ( 'NONE', #10169 ) ;
#1265 = AXIS2_PLACEMENT_3D ( 'NONE', #61, #11555, #4558 ) ;
#1266 = CARTESIAN_POINT ( 'NONE',  ( -92.38795325112826617, 38.26834323650999181, 8.000000000000000000 ) ) ;
#1267 = FACE_OUTER_BOUND ( 'NONE', #14581, .T. ) ;
#1268 = CARTESIAN_POINT ( 'NONE',  ( 2.742827927723424875, 3.035229711105287276, -3.433252694550964268 ) ) ;
#1269 = DIRECTION ( 'NONE',  ( 1.000000000000000000, 0.000000000000000000, 0.000000000000000000 ) ) ;
#1270 = DIRECTION ( 'NONE',  ( 0.000000000000000000, 0.000000000000000000, 1.000000000000000000 ) ) ;
#1271 = ORIENTED_EDGE ( 'NONE', *, *, #7692, .T. ) ;
#1272 = DIRECTION ( 'NONE',  ( -0.000000000000000000, -0.000000000000000000, -1.000000000000000000 ) ) ;
#1273 = EDGE_CURVE ( 'NONE', #11793, #11847, #5855, .T. ) ;
#1274 = ORIENTED_EDGE ( 'NONE', *, *, #11236, .T. ) ;
#1275 = AXIS2_PLACEMENT_3D ( 'NONE', #5796, #12652, #14860 ) ;
#1276 = ORIENTED_EDGE ( 'NONE', *, *, #13026, .T. ) ;
#1277 = VERTEX_POINT ( 'NONE', #11330 ) ;
#1278 = DIRECTION ( 'NONE',  ( 0.000000000000000000, 0.000000000000000000, -1.000000000000000000 ) ) ;
#1279 = CARTESIAN_POINT ( 'NONE',  ( -39.66766701456180755, -30.43807145043597373, -8.000000000000000000 ) ) ;
#1280 = CIRCLE ( 'NONE', #2973, 50.00000000000000000 ) ;
#1281 = ORIENTED_EDGE ( 'NONE', *, *, #2771, .T. ) ;
#1282 = VERTEX_POINT ( 'NONE', #14597 ) ;
#1283 = CARTESIAN_POINT ( 'NONE',  ( -37.12029293941250074, 89.61631465359532456, 8.000000000000000000 ) ) ;
#1284 = ORIENTED_EDGE ( 'NONE', *, *, #43, .F. ) ;
#1285 = AXIS2_PLACEMENT_3D ( 'NONE', #963, #8998, #5583 ) ;
#1286 = CARTESIAN_POINT ( 'NONE',  ( 30.80502811811196295, 49.00442420936003174, 8.000000000000000000 ) ) ;
#1287 = FACE_OUTER_BOUND ( 'NONE', #9145, .T. ) ;
#1288 = FACE_OUTER_BOUND ( 'NONE', #9095, .T. ) ;
#1290 = EDGE_LOOP ( 'NONE', ( #7125, #7121, #500, #6084, #514, #11735, #1897, #13046 ) ) ;
#1289 = EDGE_CURVE ( 'NONE', #5235, #3918, #3659, .T. ) ;
#1291 = VECTOR ( 'NONE', #5295, 1000.000000000000000 ) ;
#1292 = DIRECTION ( 'NONE',  ( 0.2941176470588243164, 0.9557692240748186796, 0.000000000000000000 ) ) ;
#1293 = DIRECTION ( 'NONE',  ( -1.000000000000000000, 0.000000000000000000, 0.000000000000000000 ) ) ;
#1294 = EDGE_CURVE ( 'NONE', #4446, #1777, #1831, .T. ) ;
#1295 = ORIENTED_EDGE ( 'NONE', *, *, #2095, .F. ) ;
#1296 = CARTESIAN_POINT ( 'NONE',  ( 0.000000000000000000, 0.000000000000000000, 14.49999999999999822 ) ) ;
#1297 = AXIS2_PLACEMENT_3D ( 'NONE', #9572, #1395, #5100 ) ;
#1298 = ORIENTED_EDGE ( 'NONE', *, *, #2210, .F. ) ;
#1299 = EDGE_CURVE ( 'NONE', #12729, #12788, #5591, .T. ) ;
#1300 = VECTOR ( 'NONE', #6477, 1000.000000000000000 ) ;
#1301 = DIRECTION ( 'NONE',  ( 0.000000000000000000, 0.000000000000000000, 1.000000000000000000 ) ) ;
#1302 = DIRECTION ( 'NONE',  ( 0.000000000000000000, 0.000000000000000000, -1.000000000000000000 ) ) ;
#1303 = AXIS2_PLACEMENT_3D ( 'NONE', #10832, #10985, #4009 ) ;
#1304 = CARTESIAN_POINT ( 'NONE',  ( -24.98583958711379083, -30.74264578624812927, -25.50000000000000355 ) ) ;
#1305 = CARTESIAN_POINT ( 'NONE',  ( -8.791121401460923579, 106.6383652286473023, 19.83320147728688454 ) ) ;
#1306 = DIRECTION ( 'NONE',  ( -1.000000000000000000, 0.000000000000000000, 0.000000000000000000 ) ) ;
#1307 = DIRECTION ( 'NONE',  ( -1.000000000000000000, 0.000000000000000000, 0.000000000000000000 ) ) ;
#1308 = ITEM_DEFINED_TRANSFORMATION ( 'NONE', 'NONE', #10164,  #5108 ) ;
#1309 = EDGE_CURVE ( 'NONE', #2752, #915, #12866, .T. ) ;
#1310 = CIRCLE ( 'NONE', #3500, 60.50000000000000000 ) ;
#1311 = DIRECTION ( 'NONE',  ( 0.000000000000000000, 0.000000000000000000, 1.000000000000000000 ) ) ;
#1312 = VECTOR ( 'NONE', #6383, 1000.000000000000000 ) ;
#1313 = ORIENTED_EDGE ( 'NONE', *, *, #7794, .T. ) ;
#1314 = DIRECTION ( 'NONE',  ( 0.000000000000000000, 0.000000000000000000, 1.000000000000000000 ) ) ;
#1315 = LINE ( 'NONE', #8211, #7602 ) ;
#1316 = DIRECTION ( 'NONE',  ( -0.000000000000000000, -0.000000000000000000, 1.000000000000000000 ) ) ;
#1317 = FACE_OUTER_BOUND ( 'NONE', #9566, .T. ) ;
#1318 = ORIENTED_EDGE ( 'NONE', *, *, #9870, .T. ) ;
#1319 = AXIS2_PLACEMENT_3D ( 'NONE', #8752, #3075, #12405 ) ;
#1320 = CONICAL_SURFACE ( 'NONE', #2784, 2.500000000000000888, 0.9599310885968785900 ) ;
#1321 = VECTOR ( 'NONE', #14261, 1000.000000000000000 ) ;
#1322 = LINE ( 'NONE', #2374, #2219 ) ;
#1323 = AXIS2_PLACEMENT_3D ( 'NONE', #11820, #9877, #9374 ) ;
#1324 = ORIENTED_EDGE ( 'NONE', *, *, #10190, .T. ) ;
#1325 =( BOUNDED_SURFACE ( )  B_SPLINE_SURFACE ( 3, 2, ( 
 ( #9176, #9022, #11558 ),
 ( #10248, #923, #7033 ),
 ( #13751, #5760, #2346 ),
 ( #993, #9935, #7957 ),
 ( #12600, #4631, #6963 ),
 ( #13903, #8114, #1212 ) ),
 .UNSPECIFIED., .F., .F., .F. ) 
 B_SPLINE_SURFACE_WITH_KNOTS ( ( 4, 2, 4 ),
 ( 3, 3 ),
 ( 0.02032853247518125531, 0.02278863295364820865, 0.02524873343211516200 ),
 ( 0.000000000000000000, 1.000000000000000000 ),
 .UNSPECIFIED. ) 
 GEOMETRIC_REPRESENTATION_ITEM ( )  RATIONAL_B_SPLINE_SURFACE ( (
 ( 1.000000000000000000, 0.8047781615896836271, 1.000000000000000000),
 ( 1.000000000000000000, 0.8123767586288900278, 1.000000000000000000),
 ( 1.000000000000000000, 0.8190662415564865517, 1.000000000000000000),
 ( 1.000000000000000000, 0.8192361015668555568, 1.000000000000000000),
 ( 1.000000000000000000, 0.8126135807104253317, 1.000000000000000000),
 ( 1.000000000000000000, 0.8047712338318587788, 1.000000000000000000) ) ) 
 REPRESENTATION_ITEM ( '' )  SURFACE ( )  );
#1326 = CARTESIAN_POINT ( 'NONE',  ( -2.687328764639638212, 3.067272167851283982, -0.05923475698270262019 ) ) ;
#1327 = CARTESIAN_POINT ( 'NONE',  ( -3.999999999999997335, 0.1981133338132461397, 2.803114366780232176E-15 ) ) ;
#1328 = FACE_OUTER_BOUND ( 'NONE', #2402, .T. ) ;
#1329 = DIRECTION ( 'NONE',  ( -0.000000000000000000, -0.000000000000000000, 1.000000000000000000 ) ) ;
#1330 = CIRCLE ( 'NONE', #11761, 3.000000000000002665 ) ;
#1331 = VERTEX_POINT ( 'NONE', #13372 ) ;
#1332 = VECTOR ( 'NONE', #11907, 1000.000000000000000 ) ;
#1333 = CARTESIAN_POINT ( 'NONE',  ( -42.04772703543551415, -32.26435573746212526, -8.000000000000000000 ) ) ;
#1334 = DIRECTION ( 'NONE',  ( 0.000000000000000000, 1.000000000000000000, 0.000000000000000000 ) ) ;
#1335 = AXIS2_PLACEMENT_3D ( 'NONE', #7355, #7432, #7205 ) ;
#1336 = LINE ( 'NONE', #4756, #9747 ) ;
#1337 = ADVANCED_FACE ( 'NONE', ( #855 ), #774, .T. ) ;
#1338 = VERTEX_POINT ( 'NONE', #13591 ) ;
#1339 = ADVANCED_FACE ( 'NONE', ( #11098 ), #7816, .T. ) ;
#1340 = ORIENTED_EDGE ( 'NONE', *, *, #10068, .F. ) ;
#1341 = CIRCLE ( 'NONE', #4739, 10.00000000000000178 ) ;
#1342 = EDGE_LOOP ( 'NONE', ( #5577, #448 ) ) ;
#1343 = AXIS2_PLACEMENT_3D ( 'NONE', #2632, #359, #7409 ) ;
#1344 = CARTESIAN_POINT ( 'NONE',  ( 30.80502811811196295, 49.00442420936003174, -10.50000000000000000 ) ) ;
#1345 = AXIS2_PLACEMENT_3D ( 'NONE', #4265, #12374, #12307 ) ;
#1346 = CARTESIAN_POINT ( 'NONE',  ( -25.99999999999971223, -45.89934640057541060, -10.50000000000000000 ) ) ;
#1347 = DIRECTION ( 'NONE',  ( 1.000000000000000000, 0.000000000000000000, 0.000000000000000000 ) ) ;
#1348 = CARTESIAN_POINT ( 'NONE',  ( 0.000000000000000000, 0.000000000000000000, 0.000000000000000000 ) ) ;
#1349 = CARTESIAN_POINT ( 'NONE',  ( 32.39328945492017198, -42.64958156413663914, -10.50000000000000000 ) ) ;
#1350 = EDGE_LOOP ( 'NONE', ( #12664, #5339, #9575, #4664, #14640 ) ) ;
#1351 = DIRECTION ( 'NONE',  ( 0.000000000000000000, 0.000000000000000000, -1.000000000000000000 ) ) ;
#1352 = ORIENTED_EDGE ( 'NONE', *, *, #14789, .F. ) ;
#1353 = ADVANCED_FACE ( 'NONE', ( #5253 ), #5402, .F. ) ;
#1354 = ORIENTED_EDGE ( 'NONE', *, *, #1522, .F. ) ;
#1355 = CARTESIAN_POINT ( 'NONE',  ( 32.26435573746228158, -42.04772703543541468, -10.50000000000000000 ) ) ;
#1356 = DIRECTION ( 'NONE',  ( -1.000000000000000000, 0.000000000000000000, 0.000000000000000000 ) ) ;
#1357 = AXIS2_PLACEMENT_3D ( 'NONE', #14345, #1744, #1888 ) ;
#1358 = DIRECTION ( 'NONE',  ( -1.000000000000000000, 0.000000000000000000, 0.000000000000000000 ) ) ;
#1359 = ADVANCED_FACE ( 'NONE', ( #14672 ), #12463, .T. ) ;
#1360 = ORIENTED_EDGE ( 'NONE', *, *, #559, .F. ) ;
#1361 = ORIENTED_EDGE ( 'NONE', *, *, #9655, .T. ) ;
#1362 = CARTESIAN_POINT ( 'NONE',  ( 12.39897948556635754, 73.96800191783272282, -16.00000000000000000 ) ) ;
#1363 = ORIENTED_EDGE ( 'NONE', *, *, #5786, .F. ) ;
#1364 = FACE_OUTER_BOUND ( 'NONE', #7802, .T. ) ;
#1365 = FACE_OUTER_BOUND ( 'NONE', #5975, .T. ) ;
#1366 = VECTOR ( 'NONE', #1205, 1000.000000000000000 ) ;
#1367 = PLANE ( 'NONE',  #7399 ) ;
#1368 = CARTESIAN_POINT ( 'NONE',  ( -47.21331623427138879, -33.48561063518577896, -13.00000000000000178 ) ) ;
#1369 = DIRECTION ( 'NONE',  ( 0.000000000000000000, 0.000000000000000000, 1.000000000000000000 ) ) ;
#1370 = DIRECTION ( 'NONE',  ( 0.000000000000000000, 0.000000000000000000, -1.000000000000000000 ) ) ;
#1371 = EDGE_LOOP ( 'NONE', ( #10075, #6028, #9501, #13452, #10870, #9766, #4151, #3921 ) ) ;
#1372 = CARTESIAN_POINT ( 'NONE',  ( -3.999999999999996447, 1.539600717838995880, -3.300726591567077595 ) ) ;
#1373 = ORIENTED_EDGE ( 'NONE', *, *, #8469, .F. ) ;
#1374 = AXIS2_PLACEMENT_3D ( 'NONE', #10651, #338, #7159 ) ;
#1375 = ORIENTED_EDGE ( 'NONE', *, *, #3011, .T. ) ;
#1376 = EDGE_CURVE ( 'NONE', #10004, #13345, #9463, .T. ) ;
#1377 = ORIENTED_EDGE ( 'NONE', *, *, #11829, .T. ) ;
#1378 = EDGE_CURVE ( 'NONE', #11847, #14140, #14209, .T. ) ;
#1379 = CARTESIAN_POINT ( 'NONE',  ( 20.00000000000000000, 2.449293598294706513E-15, 13.00000000000000178 ) ) ;
#1380 = EDGE_CURVE ( 'NONE', #362, #8812, #1511, .T. ) ;
#1381 = VERTEX_POINT ( 'NONE', #13829 ) ;
#1382 = CARTESIAN_POINT ( 'NONE',  ( 2.449848172108559208, 3.432307619358739625, -3.503702292528904749 ) ) ;
#1383 = DIRECTION ( 'NONE',  ( 0.000000000000000000, 0.000000000000000000, -1.000000000000000000 ) ) ;
#1384 = AXIS2_PLACEMENT_3D ( 'NONE', #5807, #10597, #4765 ) ;
#1385 = LINE ( 'NONE', #12014, #5359 ) ;
#1386 = FACE_OUTER_BOUND ( 'NONE', #1406, .T. ) ;
#1387 = AXIS2_PLACEMENT_3D ( 'NONE', #12025, #13293, #10862 ) ;
#1388 = CARTESIAN_POINT ( 'NONE',  ( 12.39897948556635754, 94.18739463280904545, -16.00000000000000000 ) ) ;
#1389 = ORIENTED_EDGE ( 'NONE', *, *, #14735, .T. ) ;
#1390 = EDGE_CURVE ( 'NONE', #12633, #3199, #2202, .T. ) ;
#1391 = CARTESIAN_POINT ( 'NONE',  ( 2.449293598294700991E-16, -97.00000000000000000, -8.000000000000000000 ) ) ;
#1392 = VERTEX_POINT ( 'NONE', #12609 ) ;
#1393 = DIRECTION ( 'NONE',  ( -1.000000000000000000, 0.000000000000000000, 0.000000000000000000 ) ) ;
#1394 = FACE_OUTER_BOUND ( 'NONE', #1945, .T. ) ;
#1395 = DIRECTION ( 'NONE',  ( 0.000000000000000000, 0.000000000000000000, 1.000000000000000000 ) ) ;
#1396 = EDGE_CURVE ( 'NONE', #6857, #10287, #13355, .T. ) ;
#1397 = LINE ( 'NONE', #326, #1079 ) ;
#1398 = EDGE_CURVE ( 'NONE', #2051, #7460, #2433, .T. ) ;
#1399 = ORIENTED_EDGE ( 'NONE', *, *, #6844, .F. ) ;
#1400 = DIRECTION ( 'NONE',  ( 0.000000000000000000, 0.000000000000000000, 1.000000000000000000 ) ) ;
#1401 = VERTEX_POINT ( 'NONE', #6903 ) ;
#1402 = CYLINDRICAL_SURFACE ( 'NONE', #14803, 52.50000000000000711 ) ;
#1403 = DIRECTION ( 'NONE',  ( -0.000000000000000000, -0.000000000000000000, 1.000000000000000000 ) ) ;
#1404 = DIRECTION ( 'NONE',  ( 1.000000000000000000, 0.000000000000000000, 0.000000000000000000 ) ) ;
#1405 = DIRECTION ( 'NONE',  ( 0.000000000000000000, 0.000000000000000000, 1.000000000000000000 ) ) ;
#1406 = EDGE_LOOP ( 'NONE', ( #12272, #2635, #12944, #14162 ) ) ;
#1407 = DIRECTION ( 'NONE',  ( -1.000000000000000000, 0.000000000000000000, 0.000000000000000000 ) ) ;
#1408 = DIRECTION ( 'NONE',  ( -1.000000000000000000, 0.000000000000000000, 0.000000000000000000 ) ) ;
#1409 = CARTESIAN_POINT ( 'NONE',  ( -36.62029293941440500, -89.61631465359452875, -10.50000000000000000 ) ) ;
#1410 = ORIENTED_EDGE ( 'NONE', *, *, #7578, .T. ) ;
#1411 = EDGE_LOOP ( 'NONE', ( #2059, #8484, #7620, #10464, #10607, #1739 ) ) ;
#1412 = CIRCLE ( 'NONE', #2135, 59.50000000000000000 ) ;
#1413 = DIRECTION ( 'NONE',  ( 1.000000000000000000, 0.000000000000000000, 0.000000000000000000 ) ) ;
#1414 = DIRECTION ( 'NONE',  ( 0.000000000000000000, 0.000000000000000000, -1.000000000000000000 ) ) ;
#1415 = CARTESIAN_POINT ( 'NONE',  ( 0.5449313310646723973, 4.304185902836962896, -3.316620875263447399 ) ) ;
#1416 = FILL_AREA_STYLE_COLOUR ( '', #8948 ) ;
#1417 = ADVANCED_FACE ( 'NONE', ( #8194 ), #12831, .F. ) ;
#1418 = FACE_OUTER_BOUND ( 'NONE', #12269, .T. ) ;
#1419 = ORIENTED_EDGE ( 'NONE', *, *, #11505, .F. ) ;
#1420 = ORIENTED_EDGE ( 'NONE', *, *, #10091, .T. ) ;
#1421 = ORIENTED_EDGE ( 'NONE', *, *, #8740, .F. ) ;
#1422 = CARTESIAN_POINT ( 'NONE',  ( 55.00000000000000711, 0.000000000000000000, 2.055000000000000160 ) ) ;
#1423 = DIRECTION ( 'NONE',  ( 0.000000000000000000, 0.000000000000000000, -1.000000000000000000 ) ) ;
#1424 = CARTESIAN_POINT ( 'NONE',  ( 12.86891638962116247, -56.43380494354001087, -13.00000000000000178 ) ) ;
#1425 = ORIENTED_EDGE ( 'NONE', *, *, #8652, .F. ) ;
#1426 = ORIENTED_EDGE ( 'NONE', *, *, #4047, .T. ) ;
#1427 = FACE_OUTER_BOUND ( 'NONE', #7018, .T. ) ;
#1428 = ORIENTED_EDGE ( 'NONE', *, *, #9477, .F. ) ;
#1429 = DIRECTION ( 'NONE',  ( -1.000000000000000000, 0.000000000000000000, 0.000000000000000000 ) ) ;
#1430 = CARTESIAN_POINT ( 'NONE',  ( -10.21287289150292921, 74.30275811153845211, 19.23918552186208686 ) ) ;
#1431 = EDGE_CURVE ( 'NONE', #5810, #5135, #74, .T. ) ;
#1432 = CARTESIAN_POINT ( 'NONE',  ( 0.5276280594147310099, -4.314175951381931995, -3.320322319201609584 ) ) ;
#1433 = DIRECTION ( 'NONE',  ( -0.000000000000000000, -0.000000000000000000, -1.000000000000000000 ) ) ;
#1434 = EDGE_CURVE ( 'NONE', #4396, #13798, #4339, .T. ) ;
#1435 = EDGE_CURVE ( 'NONE', #2940, #9073, #12819, .T. ) ;
#1436 = ORIENTED_EDGE ( 'NONE', *, *, #4515, .F. ) ;
#1437 = CYLINDRICAL_SURFACE ( 'NONE', #6308, 5.000000000000000888 ) ;
#1438 = FACE_OUTER_BOUND ( 'NONE', #9792, .T. ) ;
#1439 = ORIENTED_EDGE ( 'NONE', *, *, #9429, .F. ) ;
#1440 = FACE_OUTER_BOUND ( 'NONE', #2596, .T. ) ;
#1441 = VERTEX_POINT ( 'NONE', #9258 ) ;
#1443 = ORIENTED_EDGE ( 'NONE', *, *, #6310, .F. ) ;
#1442 = APPLICATION_CONTEXT ( 'automotive_design' ) ;
#1444 = CARTESIAN_POINT ( 'NONE',  ( 45.89934640057532533, -26.49999999999987566, 8.000000000000000000 ) ) ;
#1445 = VERTEX_POINT ( 'NONE', #5618 ) ;
#1446 = CARTESIAN_POINT ( 'NONE',  ( -20.00000000000000000, 2.449293598294706513E-15, -25.50000000000000355 ) ) ;
#1447 = CARTESIAN_POINT ( 'NONE',  ( 31.72333741318945144, 102.1879147510518777, -12.61437971294004434 ) ) ;
#1448 = DIRECTION ( 'NONE',  ( 0.000000000000000000, 0.000000000000000000, 1.000000000000000000 ) ) ;
#1449 = CARTESIAN_POINT ( 'NONE',  ( 0.000000000000000000, 0.000000000000000000, -8.000000000000000000 ) ) ;
#1450 = DIRECTION ( 'NONE',  ( -0.000000000000000000, -0.000000000000000000, -1.000000000000000000 ) ) ;
#1451 = VECTOR ( 'NONE', #4253, 1000.000000000000114 ) ;
#1452 = DIRECTION ( 'NONE',  ( 1.000000000000000000, 0.000000000000000000, -0.000000000000000000 ) ) ;
#1453 = VERTEX_POINT ( 'NONE', #10254 ) ;
#1454 = CIRCLE ( 'NONE', #11398, 44.89637028918152595 ) ;
#1455 = FACE_OUTER_BOUND ( 'NONE', #10690, .T. ) ;
#1456 = ORIENTED_EDGE ( 'NONE', *, *, #1154, .T. ) ;
#1457 = ADVANCED_FACE ( 'NONE', ( #14972 ), #9334, .F. ) ;
#1458 = DIRECTION ( 'NONE',  ( 1.000000000000000000, -2.664535259100375697E-15, 0.000000000000000000 ) ) ;
#1459 = DIRECTION ( 'NONE',  ( -0.000000000000000000, -0.000000000000000000, -1.000000000000000000 ) ) ;
#1460 = EDGE_CURVE ( 'NONE', #9900, #5810, #11616, .T. ) ;
#1461 = FACE_OUTER_BOUND ( 'NONE', #12852, .T. ) ;
#1462 = CIRCLE ( 'NONE', #11912, 0.5000000000000004441 ) ;
#1463 = LINE ( 'NONE', #11869, #7105 ) ;
#1464 = ORIENTED_EDGE ( 'NONE', *, *, #14610, .F. ) ;
#1465 = AXIS2_PLACEMENT_3D ( 'NONE', #1014, #5557, #7829 ) ;
#1466 = PLANE ( 'NONE',  #7745 ) ;
#1467 = VECTOR ( 'NONE', #1991, 1000.000000000000000 ) ;
#1468 = VERTEX_POINT ( 'NONE', #13909 ) ;
#1469 = DIRECTION ( 'NONE',  ( 0.000000000000000000, 0.000000000000000000, 1.000000000000000000 ) ) ;
#1470 = DIRECTION ( 'NONE',  ( 0.000000000000000000, 0.000000000000000000, 1.000000000000000000 ) ) ;
#1471 = CARTESIAN_POINT ( 'NONE',  ( -90.10640870805754332, -37.02125851216322872, -10.50000000000000000 ) ) ;
#1472 = DIRECTION ( 'NONE',  ( 0.000000000000000000, 0.000000000000000000, 1.000000000000000000 ) ) ;
#1473 = STYLED_ITEM ( 'NONE', ( #1754 ), #9171 ) ;
#1474 = EDGE_CURVE ( 'NONE', #3015, #13429, #11565, .T. ) ;
#1475 = AXIS2_PLACEMENT_3D ( 'NONE', #6663, #2120, #11319 ) ;
#1476 = ORIENTED_EDGE ( 'NONE', *, *, #11787, .F. ) ;
#1477 = EDGE_CURVE ( 'NONE', #6265, #967, #4566, .T. ) ;
#1478 = CARTESIAN_POINT ( 'NONE',  ( 30.80502811811196295, 49.00442420936003174, -13.00000000000000178 ) ) ;
#1479 = AXIS2_PLACEMENT_3D ( 'NONE', #3814, #10710, #7130 ) ;
#1480 = DIRECTION ( 'NONE',  ( 0.000000000000000000, 0.000000000000000000, 1.000000000000000000 ) ) ;
#1481 = VECTOR ( 'NONE', #1957, 1000.000000000000000 ) ;
#1482 = CARTESIAN_POINT ( 'NONE',  ( -22.05882352941176450, 71.68269180561142662, -16.00000000000000000 ) ) ;
#1483 = VERTEX_POINT ( 'NONE', #10476 ) ;
#1484 = ADVANCED_FACE ( 'NONE', ( #4641 ), #3503, .F. ) ;
#1485 = VERTEX_POINT ( 'NONE', #3175 ) ;
#1486 = CIRCLE ( 'NONE', #10218, 0.5000000000000004441 ) ;
#1487 = LINE ( 'NONE', #13257, #2797 ) ;
#1488 = FACE_OUTER_BOUND ( 'NONE', #7782, .T. ) ;
#1489 = AXIS2_PLACEMENT_3D ( 'NONE', #14541, #5279, #3999 ) ;
#1490 = CARTESIAN_POINT ( 'NONE',  ( 0.000000000000000000, 0.000000000000000000, 8.000000000000000000 ) ) ;
#1491 = AXIS2_PLACEMENT_3D ( 'NONE', #919, #5537, #12679 ) ;
#1492 = CARTESIAN_POINT ( 'NONE',  ( 89.33979373934423052, -36.70371619500547666, -13.00000000000000178 ) ) ;
#1493 = CARTESIAN_POINT ( 'NONE',  ( 0.000000000000000000, 0.000000000000000000, 0.000000000000000000 ) ) ;
#1494 = CYLINDRICAL_SURFACE ( 'NONE', #13473, 3.000000000000002665 ) ;
#1495 = VERTEX_POINT ( 'NONE', #2031 ) ;
#1496 = ORIENTED_EDGE ( 'NONE', *, *, #13694, .T. ) ;
#1497 = EDGE_CURVE ( 'NONE', #7269, #5893, #5542, .T. ) ;
#1498 = EDGE_LOOP ( 'NONE', ( #1221, #1723 ) ) ;
#1499 = CARTESIAN_POINT ( 'NONE',  ( 9.706953719245472456, 57.06275842387054098, -8.000000000000000000 ) ) ;
#1500 = DIRECTION ( 'NONE',  ( -1.000000000000000000, 0.000000000000000000, 0.000000000000000000 ) ) ;
#1501 = AXIS2_PLACEMENT_3D ( 'NONE', #4653, #2297, #5929 ) ;
#1502 = CARTESIAN_POINT ( 'NONE',  ( -9.714003807513881483, -53.63365512954690217, -8.000000000000000000 ) ) ;
#1503 = ORIENTED_EDGE ( 'NONE', *, *, #7814, .T. ) ;
#1504 = AXIS2_PLACEMENT_3D ( 'NONE', #9059, #13707, #3083 ) ;
#1505 = ORIENTED_EDGE ( 'NONE', *, *, #3299, .T. ) ;
#1506 = DIRECTION ( 'NONE',  ( 0.000000000000000000, 0.000000000000000000, -1.000000000000000000 ) ) ;
#1507 = ORIENTED_EDGE ( 'NONE', *, *, #302, .T. ) ;
#1508 = CYLINDRICAL_SURFACE ( 'NONE', #257, 5.000000000000000888 ) ;
#1509 = AXIS2_PLACEMENT_3D ( 'NONE', #4880, #14137, #11641 ) ;
#1510 = CARTESIAN_POINT ( 'NONE',  ( -0.02448733951239507114, -4.877042772274745808, -3.751161874094030679 ) ) ;
#1511 = B_SPLINE_CURVE_WITH_KNOTS ( 'NONE', 3,
 ( #2285, #12765, #10331, #2130, #7965, #12687 ),
 .UNSPECIFIED., .F., .F.,
 ( 4, 2, 4 ),
 ( 0.002452478801916377609, 0.003676905084148009151, 0.004901331366379640259 ),
 .UNSPECIFIED. ) ;
#1512 = DIRECTION ( 'NONE',  ( 1.000000000000000000, 0.000000000000000000, 0.000000000000000000 ) ) ;
#1513 = DIRECTION ( 'NONE',  ( 1.000000000000000000, 0.000000000000000000, 0.000000000000000000 ) ) ;
#1514 = AXIS2_PLACEMENT_3D ( 'NONE', #12940, #2532, #13860 ) ;
#1515 = EDGE_LOOP ( 'NONE', ( #3520, #12611, #7633, #1038, #14892, #4994, #4703, #9659, #13442, #13541, #14353, #12220 ) ) ;
#1516 = DIRECTION ( 'NONE',  ( 0.000000000000000000, 0.000000000000000000, 1.000000000000000000 ) ) ;
#1517 = VERTEX_POINT ( 'NONE', #7714 ) ;
#1518 = EDGE_CURVE ( 'NONE', #10622, #11548, #7942, .T. ) ;
#1519 = AXIS2_PLACEMENT_3D ( 'NONE', #1871, #14937, #9370 ) ;
#1520 = ORIENTED_EDGE ( 'NONE', *, *, #9716, .T. ) ;
#1521 = DIRECTION ( 'NONE',  ( -0.000000000000000000, -0.000000000000000000, 1.000000000000000000 ) ) ;
#1522 = EDGE_CURVE ( 'NONE', #14486, #4561, #13019, .T. ) ;
#1523 = CARTESIAN_POINT ( 'NONE',  ( 0.000000000000000000, -2.357898499370437939, 0.000000000000000000 ) ) ;
#1524 = CIRCLE ( 'NONE', #13901, 3.000000000000002665 ) ;
#1525 = CARTESIAN_POINT ( 'NONE',  ( 0.000000000000000000, 0.000000000000000000, -13.50000000000000178 ) ) ;
#1526 = CARTESIAN_POINT ( 'NONE',  ( -68.68541276968778675, 69.08004447556137961, -10.50000000000000000 ) ) ;
#1527 = CARTESIAN_POINT ( 'NONE',  ( 0.000000000000000000, 0.000000000000000000, 31.00000000000000000 ) ) ;
#1528 = DIRECTION ( 'NONE',  ( 1.000000000000000000, 0.000000000000000000, 0.000000000000000000 ) ) ;
#1529 = EDGE_CURVE ( 'NONE', #5666, #3662, #7649, .T. ) ;
#1530 = DIRECTION ( 'NONE',  ( 0.000000000000000000, 0.000000000000000000, -1.000000000000000000 ) ) ;
#1531 = CIRCLE ( 'NONE', #11482, 2.500000000000000444 ) ;
#1532 = ORIENTED_EDGE ( 'NONE', *, *, #3615, .F. ) ;
#1533 = DIRECTION ( 'NONE',  ( 1.000000000000000000, 0.000000000000000000, 0.000000000000000000 ) ) ;
#1534 = ORIENTED_EDGE ( 'NONE', *, *, #8925, .T. ) ;
#1535 = EDGE_CURVE ( 'NONE', #6344, #3532, #3101, .T. ) ;
#1536 = CARTESIAN_POINT ( 'NONE',  ( 37.12029293941315444, -89.61631465359504034, -13.00000000000000178 ) ) ;
#1537 = DIRECTION ( 'NONE',  ( 0.000000000000000000, 0.000000000000000000, 1.000000000000000000 ) ) ;
#1538 = AXIS2_PLACEMENT_3D ( 'NONE', #9156, #8237, #5669 ) ;
#1539 = CARTESIAN_POINT ( 'NONE',  ( 0.000000000000000000, 0.000000000000000000, -10.50000000000000000 ) ) ;
#1540 = ADVANCED_FACE ( 'NONE', ( #826 ), #3326, .T. ) ;
#1541 = DIRECTION ( 'NONE',  ( -1.000000000000000000, 0.000000000000000000, 0.000000000000000000 ) ) ;
#1542 = VERTEX_POINT ( 'NONE', #10080 ) ;
#1543 = CIRCLE ( 'NONE', #14391, 5.000000000000001776 ) ;
#1544 = ORIENTED_EDGE ( 'NONE', *, *, #2587, .F. ) ;
#1545 = CARTESIAN_POINT ( 'NONE',  ( 0.000000000000000000, 0.000000000000000000, -13.00000000000000178 ) ) ;
#1546 = ORIENTED_EDGE ( 'NONE', *, *, #11963, .F. ) ;
#1547 = CYLINDRICAL_SURFACE ( 'NONE', #8965, 2.649999999999993694 ) ;
#1548 = DIRECTION ( 'NONE',  ( 1.000000000000000000, 0.000000000000000000, 0.000000000000000000 ) ) ;
#1549 = CIRCLE ( 'NONE', #13424, 60.50000000000000711 ) ;
#1550 = LINE ( 'NONE', #6166, #246 ) ;
#1551 = CARTESIAN_POINT ( 'NONE',  ( -19.68583958711381854, -30.74264578624812927, -25.50000000000000355 ) ) ;
#1552 = ORIENTED_EDGE ( 'NONE', *, *, #10567, .T. ) ;
#1553 = CARTESIAN_POINT ( 'NONE',  ( 18.52941176470587692, 60.21346111671358159, -31.00000000000000000 ) ) ;
#1554 = LINE ( 'NONE', #8675, #13700 ) ;
#1555 = CARTESIAN_POINT ( 'NONE',  ( 0.000000000000000000, 0.000000000000000000, 14.49999999999999822 ) ) ;
#1556 = AXIS2_PLACEMENT_3D ( 'NONE', #14823, #2357, #3 ) ;
#1557 = AXIS2_PLACEMENT_3D ( 'NONE', #12081, #5164, #389 ) ;
#1558 = AXIS2_PLACEMENT_3D ( 'NONE', #709, #5266, #8897 ) ;
#1559 = ORIENTED_EDGE ( 'NONE', *, *, #6887, .T. ) ;
#1560 = DIRECTION ( 'NONE',  ( -1.000000000000000000, 0.000000000000000000, 0.000000000000000000 ) ) ;
#1561 = ADVANCED_FACE ( 'NONE', ( #10226 ), #909, .F. ) ;
#1562 = ORIENTED_EDGE ( 'NONE', *, *, #10190, .F. ) ;
#1563 = EDGE_CURVE ( 'NONE', #13020, #12128, #972, .T. ) ;
#1564 = CARTESIAN_POINT ( 'NONE',  ( 0.000000000000000000, 4.618802153517009401, -0.5000000000000004441 ) ) ;
#1565 = EDGE_CURVE ( 'NONE', #14343, #2406, #654, .T. ) ;
#1566 = DIRECTION ( 'NONE',  ( -1.000000000000000000, 0.000000000000000000, 0.000000000000000000 ) ) ;
#1567 = CARTESIAN_POINT ( 'NONE',  ( -51.45950017607691507, 4.121772567811807342, -13.00000000000000178 ) ) ;
#1568 = CARTESIAN_POINT ( 'NONE',  ( -89.89283556784485540, 37.53686968382331202, -13.00000000000000178 ) ) ;
#1569 = AXIS2_PLACEMENT_3D ( 'NONE', #284, #2561, #9748 ) ;
#1570 = ORIENTED_EDGE ( 'NONE', *, *, #5786, .T. ) ;
#1571 = EDGE_LOOP ( 'NONE', ( #6998, #4769 ) ) ;
#1572 = EDGE_CURVE ( 'NONE', #4906, #10153, #14568, .T. ) ;
#1573 = DIRECTION ( 'NONE',  ( 0.000000000000000000, 0.000000000000000000, -1.000000000000000000 ) ) ;
#1574 = DIRECTION ( 'NONE',  ( 0.000000000000000000, 0.000000000000000000, 1.000000000000000000 ) ) ;
#1575 = DIRECTION ( 'NONE',  ( -1.000000000000000000, 0.000000000000000000, 0.000000000000000000 ) ) ;
#1576 = B_SPLINE_CURVE_WITH_KNOTS ( 'NONE', 3,
 ( #10284, #1035, #14772, #13625, #6770, #11436, #6705, #5507, #8912, #11205, #13547, #4373, #3155, #725, #8987, #888, #12498, #4304, #2091, #11355 ),
 .UNSPECIFIED., .F., .F.,
 ( 4, 2, 2, 2, 2, 2, 2, 2, 2, 4 ),
 ( 0.000000000000000000, 0.0009783702772842371286, 0.001467555415926354934, 0.001956740554568472523, 0.002935110831852707266, 0.003913481109136941576, 0.004891851386421175452, 0.005870221663705411062, 0.006848591940989644938, 0.007826962218273879682 ),
 .UNSPECIFIED. ) ;
#1577 = ORIENTED_EDGE ( 'NONE', *, *, #7452, .T. ) ;
#1578 = CIRCLE ( 'NONE', #364, 56.99999999999999289 ) ;
#1579 = ORIENTED_EDGE ( 'NONE', *, *, #3944, .F. ) ;
#1580 = DIRECTION ( 'NONE',  ( -1.000000000000000000, 0.000000000000000000, 0.000000000000000000 ) ) ;
#1581 = CIRCLE ( 'NONE', #1102, 0.5000000000000004441 ) ;
#1582 = CIRCLE ( 'NONE', #10062, 50.00000000000000000 ) ;
#1583 = AXIS2_PLACEMENT_3D ( 'NONE', #12548, #7747, #1990 ) ;
#1584 = ORIENTED_EDGE ( 'NONE', *, *, #1752, .T. ) ;
#1585 = EDGE_CURVE ( 'NONE', #490, #5159, #11376, .T. ) ;
#1586 = DIRECTION ( 'NONE',  ( 0.000000000000000000, 0.000000000000000000, -1.000000000000000000 ) ) ;
#1587 = CARTESIAN_POINT ( 'NONE',  ( 3.522875095019825764, -2.820352903225905372, -3.598441714920728618 ) ) ;
#1588 = CARTESIAN_POINT ( 'NONE',  ( 36.08010649850015739, 100.2464683348682541, 16.00000000000000000 ) ) ;
#1589 = VERTEX_POINT ( 'NONE', #9918 ) ;
#1590 = CIRCLE ( 'NONE', #7878, 59.50000000000000000 ) ;
#1591 = CARTESIAN_POINT ( 'NONE',  ( 89.12622059913255157, 37.21932736666302333, -10.50000000000000000 ) ) ;
#1592 = CARTESIAN_POINT ( 'NONE',  ( -68.58935777509570642, -68.58935777509452691, -10.50000000000000000 ) ) ;
#1593 = VERTEX_POINT ( 'NONE', #12439 ) ;
#1594 = CARTESIAN_POINT ( 'NONE',  ( 0.000000000000000000, 0.000000000000000000, 25.99999999999999645 ) ) ;
#1595 = AXIS2_PLACEMENT_3D ( 'NONE', #9325, #5829, #9393 ) ;
#1596 = ORIENTED_EDGE ( 'NONE', *, *, #11827, .T. ) ;
#1597 = VERTEX_POINT ( 'NONE', #12294 ) ;
#1598 = DIRECTION ( 'NONE',  ( 1.000000000000000000, 0.000000000000000000, 0.000000000000000000 ) ) ;
#1599 = AXIS2_PLACEMENT_3D ( 'NONE', #11133, #7551, #3090 ) ;
#1600 = ORIENTED_EDGE ( 'NONE', *, *, #3757, .F. ) ;
#1601 =( GEOMETRIC_REPRESENTATION_CONTEXT ( 3 ) GLOBAL_UNCERTAINTY_ASSIGNED_CONTEXT ( ( #8799 ) ) GLOBAL_UNIT_ASSIGNED_CONTEXT ( ( #10701, #13060, #157 ) ) REPRESENTATION_CONTEXT ( 'NONE', 'WORKASPACE' ) );
#1602 = DIRECTION ( 'NONE',  ( 0.000000000000000000, 0.000000000000000000, -1.000000000000000000 ) ) ;
#1603 = CARTESIAN_POINT ( 'NONE',  ( -89.61631465359441506, 37.12029293941468211, 8.000000000000000000 ) ) ;
#1604 = CARTESIAN_POINT ( 'NONE',  ( 38.79014761921569487, 11.74264578624841171, -28.00000000000000000 ) ) ;
#1605 = DIRECTION ( 'NONE',  ( -1.000000000000000000, 0.000000000000000000, 0.000000000000000000 ) ) ;
#1606 = CARTESIAN_POINT ( 'NONE',  ( -0.6448876103708539587, -4.246476118072355810, -0.2256878752776750596 ) ) ;
#1607 = VERTEX_POINT ( 'NONE', #1879 ) ;
#1608 = EDGE_CURVE ( 'NONE', #7966, #10117, #11074, .T. ) ;
#1609 = AXIS2_PLACEMENT_3D ( 'NONE', #6465, #13312, #874 ) ;
#1610 = FILL_AREA_STYLE ('',( #7286 ) ) ;
#1611 = ADVANCED_FACE ( 'NONE', ( #6491 ), #11304, .T. ) ;
#1612 = PRODUCT_DEFINITION_SHAPE ( 'NONE', 'NONE',  #15030 ) ;
#1613 = VERTEX_POINT ( 'NONE', #13498 ) ;
#1614 = DIRECTION ( 'NONE',  ( 0.000000000000000000, 0.000000000000000000, 1.000000000000000000 ) ) ;
#1615 = FACE_OUTER_BOUND ( 'NONE', #13971, .T. ) ;
#1616 = ORIENTED_EDGE ( 'NONE', *, *, #8934, .F. ) ;
#1617 = PLANE ( 'NONE',  #315 ) ;
#1618 = EDGE_LOOP ( 'NONE', ( #11219, #4942, #12564, #4968 ) ) ;
#1619 = DIRECTION ( 'NONE',  ( 1.000000000000000000, 1.749300984178293162E-15, 0.000000000000000000 ) ) ;
#1620 = VERTEX_POINT ( 'NONE', #12356 ) ;
#1621 = CARTESIAN_POINT ( 'NONE',  ( 0.000000000000000000, 0.000000000000000000, -5.000000000000000888 ) ) ;
#1622 = VERTEX_POINT ( 'NONE', #1955 ) ;
#1623 = EDGE_LOOP ( 'NONE', ( #8736, #90 ) ) ;
#1624 = DIRECTION ( 'NONE',  ( -0.000000000000000000, -0.000000000000000000, 1.000000000000000000 ) ) ;
#1625 = CARTESIAN_POINT ( 'NONE',  ( -15.11621636258860590, 32.12188890498260463, 16.00000000000000000 ) ) ;
#1626 = CARTESIAN_POINT ( 'NONE',  ( -23.50071946824040836, -45.96504489226015977, -13.00000000000000178 ) ) ;
#1627 = LINE ( 'NONE', #3761, #8085 ) ;
#1628 = ADVANCED_FACE ( 'NONE', ( #10146 ), #6571, .F. ) ;
#1629 = EDGE_CURVE ( 'NONE', #4561, #5144, #12198, .T. ) ;
#1630 = CARTESIAN_POINT ( 'NONE',  ( 0.000000000000000000, 0.000000000000000000, 13.00000000000000178 ) ) ;
#1631 = VERTEX_POINT ( 'NONE', #7092 ) ;
#1632 = ORIENTED_EDGE ( 'NONE', *, *, #13447, .F. ) ;
#1633 = FACE_OUTER_BOUND ( 'NONE', #5273, .T. ) ;
#1634 = DIRECTION ( 'NONE',  ( 0.000000000000000000, 0.000000000000000000, 1.000000000000000000 ) ) ;
#1635 = DIRECTION ( 'NONE',  ( -0.000000000000000000, -0.000000000000000000, 1.000000000000000000 ) ) ;
#1636 = UNCERTAINTY_MEASURE_WITH_UNIT (LENGTH_MEASURE( 1.000000000000000082E-05 ), #12959, 'distance_accuracy_value', 'NONE');
#1637 = ORIENTED_EDGE ( 'NONE', *, *, #7630, .F. ) ;
#1638 = LINE ( 'NONE', #7392, #11678 ) ;
#1639 = VERTEX_POINT ( 'NONE', #4688 ) ;
#1640 = DIRECTION ( 'NONE',  ( 0.000000000000000000, 0.000000000000000000, 1.000000000000000000 ) ) ;
#1641 = CARTESIAN_POINT ( 'NONE',  ( -26.00011991137315803, -45.91029614918952007, 10.49999999999999822 ) ) ;
#1642 = CARTESIAN_POINT ( 'NONE',  ( -12.50000000000000000, 100.2235002382176248, -79.80561291909842225 ) ) ;
#1643 = CARTESIAN_POINT ( 'NONE',  ( 36.14014761921570340, 11.74264578624841171, 14.49999999999999822 ) ) ;
#1644 = ORIENTED_EDGE ( 'NONE', *, *, #10929, .T. ) ;
#1645 = ORIENTED_EDGE ( 'NONE', *, *, #4912, .T. ) ;
#1646 = DIRECTION ( 'NONE',  ( 0.000000000000000000, 0.000000000000000000, -1.000000000000000000 ) ) ;
#1647 = DIRECTION ( 'NONE',  ( 0.000000000000000000, 0.000000000000000000, -1.000000000000000000 ) ) ;
#1648 = ADVANCED_FACE ( 'NONE', ( #4544 ), #15015, .F. ) ;
#1649 = DIRECTION ( 'NONE',  ( -1.000000000000000000, 0.000000000000000000, 0.000000000000000000 ) ) ;
#1650 = B_SPLINE_CURVE_WITH_KNOTS ( 'NONE', 3,
 ( #4000, #2781, #10595, #7402, #9446 ),
 .UNSPECIFIED., .F., .F.,
 ( 4, 1, 4 ),
 ( 0.000000000000000000, 0.002309401076758502321, 0.004618802153517004641 ),
 .UNSPECIFIED. ) ;
#1651 = ORIENTED_EDGE ( 'NONE', *, *, #699, .T. ) ;
#1652 = EDGE_CURVE ( 'NONE', #8710, #7182, #6934, .T. ) ;
#1653 = ORIENTED_EDGE ( 'NONE', *, *, #12481, .F. ) ;
#1654 = DIRECTION ( 'NONE',  ( -0.000000000000000000, -0.000000000000000000, 1.000000000000000000 ) ) ;
#1655 = ORIENTED_EDGE ( 'NONE', *, *, #12259, .F. ) ;
#1656 = CARTESIAN_POINT ( 'NONE',  ( -2.500000000000000444, 3.061616997868383634E-16, -5.000000000000000888 ) ) ;
#1657 = EDGE_CURVE ( 'NONE', #13337, #11105, #10585, .T. ) ;
#1658 = CARTESIAN_POINT ( 'NONE',  ( -0.1750025118121570633, -4.719839900820638867, -3.469254087858256508 ) ) ;
#1659 = ORIENTED_EDGE ( 'NONE', *, *, #978, .T. ) ;
#1660 = CARTESIAN_POINT ( 'NONE',  ( -45.39934640057513349, 26.50000000000019540, -13.00000000000000178 ) ) ;
#1661 = CARTESIAN_POINT ( 'NONE',  ( 32.46576781417953583, -41.59008834022656487, -13.00000000000000178 ) ) ;
#1662 = ORIENTED_EDGE ( 'NONE', *, *, #14051, .T. ) ;
#1663 = DIRECTION ( 'NONE',  ( 0.000000000000000000, 0.000000000000000000, -1.000000000000000000 ) ) ;
#1664 = EDGE_CURVE ( 'NONE', #5275, #11092, #6347, .T. ) ;
#1665 = EDGE_CURVE ( 'NONE', #13864, #5235, #13973, .T. ) ;
#1666 = ORIENTED_EDGE ( 'NONE', *, *, #6511, .F. ) ;
#1667 = AXIS2_PLACEMENT_3D ( 'NONE', #2350, #7897, #6970 ) ;
#1668 = ORIENTED_EDGE ( 'NONE', *, *, #4410, .T. ) ;
#1669 = LINE ( 'NONE', #14582, #12271 ) ;
#1670 = CARTESIAN_POINT ( 'NONE',  ( 31.47058823529413374, 102.2673069760056563, -10.99999999999999645 ) ) ;
#1671 = ADVANCED_FACE ( 'NONE', ( #9378 ), #2394, .F. ) ;
#1672 = DIRECTION ( 'NONE',  ( 0.000000000000000000, 0.000000000000000000, 1.000000000000000000 ) ) ;
#1673 = DIRECTION ( 'NONE',  ( -1.000000000000000000, 0.000000000000000000, 0.000000000000000000 ) ) ;
#1674 = CYLINDRICAL_SURFACE ( 'NONE', #8245, 0.5000000000000004441 ) ;
#1675 = ADVANCED_BREP_SHAPE_REPRESENTATION ( '', ( #4390, #5108 ), #4118 ) ;
#1676 = CARTESIAN_POINT ( 'NONE',  ( -2.649999999999989697, 38.00000000000000000, 14.49999999999999822 ) ) ;
#1677 = VERTEX_POINT ( 'NONE', #14096 ) ;
#1678 = DIRECTION ( 'NONE',  ( -0.000000000000000000, -0.000000000000000000, 1.000000000000000000 ) ) ;
#1679 = ORIENTED_EDGE ( 'NONE', *, *, #8420, .F. ) ;
#1680 = PLANE ( 'NONE',  #9851 ) ;
#1681 = AXIS2_PLACEMENT_3D ( 'NONE', #5773, #4732, #11792 ) ;
#1682 = CARTESIAN_POINT ( 'NONE',  ( 0.000000000000000000, 0.000000000000000000, 14.49999999999999822 ) ) ;
#1683 = VERTEX_POINT ( 'NONE', #9303 ) ;
#1684 = CARTESIAN_POINT ( 'NONE',  ( 25.00000000000000000, 81.24038404635960831, 16.00000000000000000 ) ) ;
#1685 = DIRECTION ( 'NONE',  ( -1.000000000000000000, 0.000000000000000000, 0.000000000000000000 ) ) ;
#1686 = ORIENTED_EDGE ( 'NONE', *, *, #7580, .F. ) ;
#1687 = CARTESIAN_POINT ( 'NONE',  ( -6.451868917687557214, -52.36539807335606156, -10.50000000000000000 ) ) ;
#1688 = ORIENTED_EDGE ( 'NONE', *, *, #8973, .F. ) ;
#1689 = VERTEX_POINT ( 'NONE', #5958 ) ;
#1690 = LINE ( 'NONE', #10643, #5808 ) ;
#1691 = DIRECTION ( 'NONE',  ( -0.000000000000000000, -0.000000000000000000, -1.000000000000000000 ) ) ;
#1692 = AXIS2_PLACEMENT_3D ( 'NONE', #1075, #3341, #10397 ) ;
#1693 = CARTESIAN_POINT ( 'NONE',  ( -34.51370081393726963, 101.0775402828204506, -15.68973407569667167 ) ) ;
#1694 = DIRECTION ( 'NONE',  ( -1.000000000000000000, 0.000000000000000000, 0.000000000000000000 ) ) ;
#1695 = CYLINDRICAL_SURFACE ( 'NONE', #7301, 20.00000000000000000 ) ;
#1696 = VERTEX_POINT ( 'NONE', #1349 ) ;
#1697 = CARTESIAN_POINT ( 'NONE',  ( 0.000000000000000000, 0.000000000000000000, 8.000000000000000000 ) ) ;
#1698 = CARTESIAN_POINT ( 'NONE',  ( 50.71110588017602794, 13.58799986788256398, -10.50000000000000000 ) ) ;
#1699 = CONICAL_SURFACE ( 'NONE', #4377, 2.055000000000000160, 0.7853981633974479459 ) ;
#1700 = UNCERTAINTY_MEASURE_WITH_UNIT (LENGTH_MEASURE( 1.000000000000000082E-05 ), #4612, 'distance_accuracy_value', 'NONE');
#1701 = CARTESIAN_POINT ( 'NONE',  ( 4.211405965630453885, 2.460463115436282600, -3.751298928144578770 ) ) ;
#1702 = EDGE_CURVE ( 'NONE', #14939, #14649, #3395, .T. ) ;
#1703 = AXIS2_PLACEMENT_3D ( 'NONE', #407, #5185, #14370 ) ;
#1704 = EDGE_CURVE ( 'NONE', #4205, #10220, #881, .T. ) ;
#1705 = AXIS2_PLACEMENT_3D ( 'NONE', #8280, #11857, #12015 ) ;
#1706 = ORIENTED_EDGE ( 'NONE', *, *, #800, .T. ) ;
#1707 = EDGE_CURVE ( 'NONE', #1207, #7016, #3786, .T. ) ;
#1708 = ADVANCED_FACE ( 'NONE', ( #3553 ), #12741, .F. ) ;
#1709 = DIRECTION ( 'NONE',  ( 0.000000000000000000, 1.000000000000000000, 1.224646799147353207E-16 ) ) ;
#1710 = ORIENTED_EDGE ( 'NONE', *, *, #11180, .F. ) ;
#1711 = DIRECTION ( 'NONE',  ( -0.000000000000000000, -0.000000000000000000, -1.000000000000000000 ) ) ;
#1712 = DIRECTION ( 'NONE',  ( 1.000000000000000000, 0.000000000000000000, 0.000000000000000000 ) ) ;
#1713 = AXIS2_PLACEMENT_3D ( 'NONE', #10559, #12773, #7126 ) ;
#1714 = CARTESIAN_POINT ( 'NONE',  ( 0.000000000000000000, 0.000000000000000000, 10.50000000000000000 ) ) ;
#1715 = CARTESIAN_POINT ( 'NONE',  ( 51.19406879332056093, 13.71740939043382745, 8.000000000000000000 ) ) ;
#1716 = DIRECTION ( 'NONE',  ( 6.123233995736766036E-17, 0.000000000000000000, 1.000000000000000000 ) ) ;
#1717 = DIRECTION ( 'NONE',  ( 0.000000000000000000, 0.000000000000000000, 1.000000000000000000 ) ) ;
#1718 = ORIENTED_EDGE ( 'NONE', *, *, #9762, .T. ) ;
#1719 = AXIS2_PLACEMENT_3D ( 'NONE', #9468, #11843, #14040 ) ;
#1720 = CARTESIAN_POINT ( 'NONE',  ( 7.500000000000000000, 59.24038404635959409, 15.00000000000000000 ) ) ;
#1721 = PLANE ( 'NONE',  #12487 ) ;
#1722 = CARTESIAN_POINT ( 'NONE',  ( 12.39897948556635754, 100.2360479454198696, -16.00000000000000000 ) ) ;
#1723 = ORIENTED_EDGE ( 'NONE', *, *, #7724, .F. ) ;
#1724 = AXIS2_PLACEMENT_3D ( 'NONE', #6819, #5763, #3576 ) ;
#1725 = AXIS2_PLACEMENT_3D ( 'NONE', #8111, #145, #4486 ) ;
#1726 = EDGE_LOOP ( 'NONE', ( #1204, #13812 ) ) ;
#1727 = DIRECTION ( 'NONE',  ( 1.000000000000000000, 0.000000000000000000, -0.000000000000000000 ) ) ;
#1728 = EDGE_CURVE ( 'NONE', #2976, #12855, #11753, .T. ) ;
#1729 = VECTOR ( 'NONE', #4913, 1000.000000000000000 ) ;
#1730 = EDGE_LOOP ( 'NONE', ( #14041, #13678 ) ) ;
#1731 = AXIS2_PLACEMENT_3D ( 'NONE', #520, #10691, #2646 ) ;
#1732 = CYLINDRICAL_SURFACE ( 'NONE', #13949, 2.500000000000000444 ) ;
#1733 = DIRECTION ( 'NONE',  ( -0.000000000000000000, 0.000000000000000000, -1.000000000000000000 ) ) ;
#1734 = DIRECTION ( 'NONE',  ( 0.000000000000000000, 0.000000000000000000, 1.000000000000000000 ) ) ;
#1735 = ORIENTED_EDGE ( 'NONE', *, *, #2918, .T. ) ;
#1737 = AXIS2_PLACEMENT_3D ( 'NONE', #9236, #9009, #12663 ) ;
#1736 = CARTESIAN_POINT ( 'NONE',  ( -49.00442420935969778, 30.80502811811250297, 8.000000000000000000 ) ) ;
#1738 = CARTESIAN_POINT ( 'NONE',  ( 6.117650515114745779, 53.20607447915232058, -10.50000000000000000 ) ) ;
#1739 = ORIENTED_EDGE ( 'NONE', *, *, #14201, .F. ) ;
#1740 = CYLINDRICAL_SURFACE ( 'NONE', #12850, 5.000000000000000888 ) ;
#1741 = CIRCLE ( 'NONE', #5614, 60.50000000000000000 ) ;
#1742 = ORIENTED_EDGE ( 'NONE', *, *, #8597, .T. ) ;
#1743 = VERTEX_POINT ( 'NONE', #1134 ) ;
#1744 = DIRECTION ( 'NONE',  ( 0.000000000000000000, 0.000000000000000000, 1.000000000000000000 ) ) ;
#1745 = CARTESIAN_POINT ( 'NONE',  ( -52.05085522212502980, 6.852625091552908110, -10.50000000000000000 ) ) ;
#1746 = EDGE_CURVE ( 'NONE', #9110, #3826, #4272, .T. ) ;
#1747 = EDGE_CURVE ( 'NONE', #10698, #10670, #8240, .T. ) ;
#1748 = CARTESIAN_POINT ( 'NONE',  ( -86.67575032682103142, -37.71449950291016506, -8.000000000000000000 ) ) ;
#1749 = DIRECTION ( 'NONE',  ( 1.000000000000000000, 0.000000000000000000, 0.000000000000000000 ) ) ;
#1750 = CYLINDRICAL_SURFACE ( 'NONE', #6767, 3.000000000000002665 ) ;
#1751 = DIRECTION ( 'NONE',  ( 0.000000000000000000, 0.000000000000000000, -1.000000000000000000 ) ) ;
#1752 = EDGE_CURVE ( 'NONE', #2510, #11469, #9346, .T. ) ;
#1753 = ORIENTED_EDGE ( 'NONE', *, *, #2736, .F. ) ;
#1754 = PRESENTATION_STYLE_ASSIGNMENT (( #395 ) ) ;
#1755 = DIRECTION ( 'NONE',  ( -1.000000000000000000, -2.775557561562867370E-14, 0.000000000000000000 ) ) ;
#1756 = AXIS2_PLACEMENT_3D ( 'NONE', #13488, #3238, #5445 ) ;
#1757 = EDGE_CURVE ( 'NONE', #8196, #13119, #2471, .T. ) ;
#1758 = CARTESIAN_POINT ( 'NONE',  ( 89.61631465359491244, 37.12029293941346708, 10.49999999999999822 ) ) ;
#1759 = CARTESIAN_POINT ( 'NONE',  ( 0.000000000000000000, 0.000000000000000000, 8.000000000000000000 ) ) ;
#1760 = PRESENTATION_LAYER_ASSIGNMENT (  '', '', ( #796 ) ) ;
#1761 = ORIENTED_EDGE ( 'NONE', *, *, #1113, .F. ) ;
#1762 = DIRECTION ( 'NONE',  ( 1.000000000000000000, 0.000000000000000000, 0.000000000000000000 ) ) ;
#1763 = CARTESIAN_POINT ( 'NONE',  ( 3.999999999999996447, 0.1981133338132474442, 2.800855612254220445E-15 ) ) ;
#1764 = ORIENTED_EDGE ( 'NONE', *, *, #4407, .F. ) ;
#1765 = DIRECTION ( 'NONE',  ( -1.000000000000000000, 0.000000000000000000, -0.000000000000000000 ) ) ;
#1766 = ORIENTED_EDGE ( 'NONE', *, *, #8510, .F. ) ;
#1767 = VECTOR ( 'NONE', #8926, 1000.000000000000000 ) ;
#1768 = AXIS2_PLACEMENT_3D ( 'NONE', #2913, #7693, #8977 ) ;
#1769 = ADVANCED_FACE ( 'NONE', ( #9449 ), #9235, .T. ) ;
#1770 = DIRECTION ( 'NONE',  ( 0.000000000000000000, 0.000000000000000000, 1.000000000000000000 ) ) ;
#1771 = DIRECTION ( 'NONE',  ( 1.000000000000000000, 0.000000000000000000, -0.000000000000000000 ) ) ;
#1772 = FACE_OUTER_BOUND ( 'NONE', #3421, .T. ) ;
#1773 = VECTOR ( 'NONE', #4961, 1000.000000000000000 ) ;
#1774 = DIRECTION ( 'NONE',  ( 1.000000000000000000, 0.000000000000000000, 0.000000000000000000 ) ) ;
#1775 = CARTESIAN_POINT ( 'NONE',  ( -26.49999999999971578, -45.89934640057541060, -13.00000000000000178 ) ) ;
#1776 = CARTESIAN_POINT ( 'NONE',  ( 0.000000000000000000, 2.357898499370430834, 0.000000000000000000 ) ) ;
#1777 = VERTEX_POINT ( 'NONE', #4916 ) ;
#1778 = CIRCLE ( 'NONE', #12446, 3.000000000000002665 ) ;
#1779 = ORIENTED_EDGE ( 'NONE', *, *, #2114, .F. ) ;
#1780 = DIRECTION ( 'NONE',  ( 0.000000000000000000, 0.000000000000000000, 1.000000000000000000 ) ) ;
#1781 = DIRECTION ( 'NONE',  ( 1.000000000000000000, 0.000000000000000000, 0.000000000000000000 ) ) ;
#1782 = AXIS2_PLACEMENT_3D ( 'NONE', #2564, #2859, #7475 ) ;
#1783 = CARTESIAN_POINT ( 'NONE',  ( 2.500000000000002220, -2.357898499370437939, 0.000000000000000000 ) ) ;
#1784 = ORIENTED_EDGE ( 'NONE', *, *, #6798, .T. ) ;
#1785 = DIRECTION ( 'NONE',  ( 1.000000000000000000, -5.329070518200751394E-15, 0.000000000000000000 ) ) ;
#1786 = AXIS2_PLACEMENT_3D ( 'NONE', #14852, #2242, #4751 ) ;
#1787 = VERTEX_POINT ( 'NONE', #9600 ) ;
#1788 = DIRECTION ( 'NONE',  ( -1.000000000000000000, 0.000000000000000000, 0.000000000000000000 ) ) ;
#1789 = CARTESIAN_POINT ( 'NONE',  ( 5.560781378645575757, 0.000000000000000000, -4.000000000000000000 ) ) ;
#1790 = EDGE_LOOP ( 'NONE', ( #682, #13336, #5718, #4831, #12440, #14577, #6256, #12647, #7287 ) ) ;
#1791 = VECTOR ( 'NONE', #11295, 1000.000000000000000 ) ;
#1792 = DIRECTION ( 'NONE',  ( 0.000000000000000000, 0.000000000000000000, -1.000000000000000000 ) ) ;
#1793 = DIRECTION ( 'NONE',  ( -0.000000000000000000, -0.000000000000000000, -1.000000000000000000 ) ) ;
#1794 = APPLICATION_PROTOCOL_DEFINITION ( 'draft international standard', 'automotive_design', 1998, #11651 ) ;
#1795 = ORIENTED_EDGE ( 'NONE', *, *, #14510, .F. ) ;
#1796 = ORIENTED_EDGE ( 'NONE', *, *, #11313, .T. ) ;
#1797 = EDGE_CURVE ( 'NONE', #14203, #697, #9116, .T. ) ;
#1798 = CARTESIAN_POINT ( 'NONE',  ( 4.938688511801393915E-15, 4.736522675502336632, -3.681124513963741851 ) ) ;
#1800 = ADVANCED_FACE ( 'NONE', ( #7469 ), #3848, .T. ) ;
#1799 = DIRECTION ( 'NONE',  ( -1.000000000000000000, 0.000000000000000000, 0.000000000000000000 ) ) ;
#1801 = VECTOR ( 'NONE', #11111, 1000.000000000000000 ) ;
#1802 = CARTESIAN_POINT ( 'NONE',  ( 42.04772703543530099, 32.26435573746242369, -10.50000000000000000 ) ) ;
#1803 = ORIENTED_EDGE ( 'NONE', *, *, #10490, .F. ) ;
#1804 = ORIENTED_EDGE ( 'NONE', *, *, #12150, .F. ) ;
#1805 = ORIENTED_EDGE ( 'NONE', *, *, #14792, .F. ) ;
#1806 = CARTESIAN_POINT ( 'NONE',  ( -33.49014761921589667, 11.74264578624790190, 14.49999999999999822 ) ) ;
#1807 = VECTOR ( 'NONE', #5376, 1000.000000000000000 ) ;
#1808 = FACE_OUTER_BOUND ( 'NONE', #7199, .T. ) ;
#1809 = VERTEX_POINT ( 'NONE', #10976 ) ;
#1810 = DIRECTION ( 'NONE',  ( 1.000000000000000000, 0.000000000000000000, 0.000000000000000000 ) ) ;
#1811 = DIRECTION ( 'NONE',  ( 1.000000000000000000, -1.953992523340275511E-14, 0.000000000000000000 ) ) ;
#1812 = EDGE_LOOP ( 'NONE', ( #10508, #10733, #3910, #9380 ) ) ;
#1813 = EDGE_CURVE ( 'NONE', #964, #3662, #8620, .T. ) ;
#1814 = CARTESIAN_POINT ( 'NONE',  ( 3.355112389629170355, -2.681727112203167174, -0.2256878752776754760 ) ) ;
#1815 = AXIS2_PLACEMENT_3D ( 'NONE', #14920, #3300, #2232 ) ;
#1816 = CIRCLE ( 'NONE', #11044, 0.5000000000000022204 ) ;
#1817 = ORIENTED_EDGE ( 'NONE', *, *, #11647, .F. ) ;
#1818 = VECTOR ( 'NONE', #8430, 1000.000000000000000 ) ;
#1819 = ORIENTED_EDGE ( 'NONE', *, *, #10834, .T. ) ;
#1820 = CARTESIAN_POINT ( 'NONE',  ( -32.08430773043616568, 95.76884182151509606, 15.34120815717650110 ) ) ;
#1821 = CARTESIAN_POINT ( 'NONE',  ( 47.21331623427115431, 33.48561063518610581, -8.000000000000000000 ) ) ;
#1822 = VECTOR ( 'NONE', #7967, 1000.000000000000000 ) ;
#1823 = DIRECTION ( 'NONE',  ( 1.000000000000000000, 0.000000000000000000, 0.000000000000000000 ) ) ;
#1824 = CARTESIAN_POINT ( 'NONE',  ( 33.49014761921571903, 11.74264578624841171, -25.50000000000000355 ) ) ;
#1825 = AXIS2_PLACEMENT_3D ( 'NONE', #13067, #6214, #11940 ) ;
#1826 = FACE_OUTER_BOUND ( 'NONE', #422, .T. ) ;
#1827 = ORIENTED_EDGE ( 'NONE', *, *, #7210, .T. ) ;
#1828 = DIRECTION ( 'NONE',  ( 0.000000000000000000, 0.000000000000000000, 1.000000000000000000 ) ) ;
#1829 = AXIS2_PLACEMENT_3D ( 'NONE', #6635, #6482, #8996 ) ;
#1830 = DIRECTION ( 'NONE',  ( 1.000000000000000000, 0.000000000000000000, 0.000000000000000000 ) ) ;
#1831 = LINE ( 'NONE', #3276, #6297 ) ;
#1832 = EDGE_CURVE ( 'NONE', #6056, #10604, #12119, .T. ) ;
#1833 = AXIS2_PLACEMENT_3D ( 'NONE', #7575, #4260, #7722 ) ;
#1834 = EDGE_CURVE ( 'NONE', #1124, #8412, #10667, .T. ) ;
#1835 = ORIENTED_EDGE ( 'NONE', *, *, #4139, .F. ) ;
#1836 = SURFACE_SIDE_STYLE ('',( #12242 ) ) ;
#1837 = ORIENTED_EDGE ( 'NONE', *, *, #1497, .F. ) ;
#1838 = CARTESIAN_POINT ( 'NONE',  ( 90.10640870805727332, 37.02125851216391794, -10.50000000000000000 ) ) ;
#1839 = VERTEX_POINT ( 'NONE', #14395 ) ;
#1840 = DIRECTION ( 'NONE',  ( -1.000000000000000000, 0.000000000000000000, 0.000000000000000000 ) ) ;
#1841 = ORIENTED_EDGE ( 'NONE', *, *, #1704, .T. ) ;
#1842 = CARTESIAN_POINT ( 'NONE',  ( 0.000000000000000000, 0.000000000000000000, 10.50000000000000000 ) ) ;
#1843 = DIRECTION ( 'NONE',  ( 0.000000000000000000, 0.000000000000000000, 1.000000000000000000 ) ) ;
#1844 = DIRECTION ( 'NONE',  ( 1.000000000000000000, 0.000000000000000000, 0.000000000000000000 ) ) ;
#1845 = AXIS2_PLACEMENT_3D ( 'NONE', #2246, #480, #1407 ) ;
#1846 = EDGE_CURVE ( 'NONE', #7769, #13374, #8379, .T. ) ;
#1847 = DIRECTION ( 'NONE',  ( -1.000000000000000000, 0.000000000000000000, 0.000000000000000000 ) ) ;
#1848 = DIRECTION ( 'NONE',  ( 1.000000000000000000, 0.000000000000000000, -0.000000000000000000 ) ) ;
#1849 = CARTESIAN_POINT ( 'NONE',  ( 18.52941176470587692, 60.21346111671358159, -16.00000000000000000 ) ) ;
#1850 = ORIENTED_EDGE ( 'NONE', *, *, #10596, .T. ) ;
#1851 = CARTESIAN_POINT ( 'NONE',  ( 0.000000000000000000, 0.000000000000000000, -28.00000000000000000 ) ) ;
#1852 = CARTESIAN_POINT ( 'NONE',  ( 12.34206246762915882, 94.19488728021195811, -16.27883530325393835 ) ) ;
#1853 = ADVANCED_FACE ( 'NONE', ( #1418 ), #279, .F. ) ;
#1854 = EDGE_CURVE ( 'NONE', #14085, #4528, #14168, .T. ) ;
#1855 = LINE ( 'NONE', #5497, #10009 ) ;
#1856 = CIRCLE ( 'NONE', #7184, 22.00000000000001421 ) ;
#1857 = PRODUCT_DEFINITION_SHAPE ( 'NONE', 'NONE',  #15037 ) ;
#1858 = ORIENTED_EDGE ( 'NONE', *, *, #8427, .T. ) ;
#1859 = CARTESIAN_POINT ( 'NONE',  ( -2.742827927723403114, -3.035229711105392081, -3.433252694550782191 ) ) ;
#1860 = ORIENTED_EDGE ( 'NONE', *, *, #2490, .T. ) ;
#1861 = AXIS2_PLACEMENT_3D ( 'NONE', #6721, #12584, #7870 ) ;
#1862 = CYLINDRICAL_SURFACE ( 'NONE', #4505, 60.49999999999999289 ) ;
#1863 = CARTESIAN_POINT ( 'NONE',  ( 2.499999999999999556, 0.000000000000000000, 3.469446951953614189E-15 ) ) ;
#1864 = DIRECTION ( 'NONE',  ( -1.000000000000000000, 0.000000000000000000, 0.000000000000000000 ) ) ;
#1865 = CARTESIAN_POINT ( 'NONE',  ( 33.48561063518626923, -47.21331623427104063, 8.000000000000000000 ) ) ;
#1866 = ORIENTED_EDGE ( 'NONE', *, *, #11969, .F. ) ;
#1867 = CIRCLE ( 'NONE', #10351, 50.00000000000000000 ) ;
#1868 = ORIENTED_EDGE ( 'NONE', *, *, #13043, .F. ) ;
#1869 = DIRECTION ( 'NONE',  ( 1.000000000000000000, 0.000000000000000000, 0.000000000000000000 ) ) ;
#1870 = DIRECTION ( 'NONE',  ( -1.000000000000000000, -4.440892098500626162E-15, 0.000000000000000000 ) ) ;
#1871 = CARTESIAN_POINT ( 'NONE',  ( 13.71740939043365337, -51.19406879332061067, -10.50000000000000000 ) ) ;
#1872 = ORIENTED_EDGE ( 'NONE', *, *, #12364, .T. ) ;
#1873 = ORIENTED_EDGE ( 'NONE', *, *, #10811, .T. ) ;
#1874 = ORIENTED_EDGE ( 'NONE', *, *, #8851, .F. ) ;
#1875 = EDGE_CURVE ( 'NONE', #914, #5501, #12055, .T. ) ;
#1876 = CARTESIAN_POINT ( 'NONE',  ( -12.39897948556635754, 100.2360479454198696, -16.00000000000000000 ) ) ;
#1877 = CARTESIAN_POINT ( 'NONE',  ( 0.000000000000000000, 0.000000000000000000, -25.50000000000000355 ) ) ;
#1878 =( NAMED_UNIT ( * ) PLANE_ANGLE_UNIT ( ) SI_UNIT ( $, .RADIAN. ) );
#1879 = CARTESIAN_POINT ( 'NONE',  ( -2.649999999999987921, 38.00000000000000000, -28.00000000000000000 ) ) ;
#1880 = ORIENTED_EDGE ( 'NONE', *, *, #4327, .F. ) ;
#1881 = DIRECTION ( 'NONE',  ( -0.000000000000000000, -0.000000000000000000, -1.000000000000000000 ) ) ;
#1882 = DIRECTION ( 'NONE',  ( 0.000000000000000000, 0.000000000000000000, 1.000000000000000000 ) ) ;
#1883 = ORIENTED_EDGE ( 'NONE', *, *, #1117, .T. ) ;
#1884 = CARTESIAN_POINT ( 'NONE',  ( 55.00000000000000711, 0.000000000000000000, 0.000000000000000000 ) ) ;
#1885 = CLOSED_SHELL ( 'NONE', ( #10718, #5433, #13573, #26, #11639, #6471, #2390, #13893, #5265, #5965, #13219, #5173, #1185, #2571, #6931, #10006, #8198, #14000, #6423, #685, #4106, #2133, #10786, #13308, #11776, #7859, #3694, #14943, #12061, #7453, #1021, #6109 ) ) ;
#1886 = VERTEX_POINT ( 'NONE', #5055 ) ;
#1887 = VERTEX_POINT ( 'NONE', #9664 ) ;
#1888 = DIRECTION ( 'NONE',  ( 1.000000000000000000, 0.000000000000000000, 0.000000000000000000 ) ) ;
#1889 = ADVANCED_FACE ( 'NONE', ( #3927 ), #1494, .T. ) ;
#1890 = EDGE_CURVE ( 'NONE', #14215, #2940, #7895, .T. ) ;
#1891 = EDGE_CURVE ( 'NONE', #14224, #2518, #9101, .T. ) ;
#1892 = CARTESIAN_POINT ( 'NONE',  ( 50.13108361037843252, 56.43380494353993271, -8.000000000000000000 ) ) ;
#1893 = AXIS2_PLACEMENT_3D ( 'NONE', #9669, #14480, #14253 ) ;
#1894 = FACE_BOUND ( 'NONE', #1623, .T. ) ;
#1895 = DIRECTION ( 'NONE',  ( 1.000000000000000000, 0.000000000000000000, 0.000000000000000000 ) ) ;
#1896 = DIRECTION ( 'NONE',  ( 0.000000000000000000, 0.000000000000000000, 1.000000000000000000 ) ) ;
#1897 = ORIENTED_EDGE ( 'NONE', *, *, #4427, .F. ) ;
#1898 = CARTESIAN_POINT ( 'NONE',  ( 0.2790467552932217044, -96.58511096861892042, -10.50000000000000000 ) ) ;
#1899 = DIRECTION ( 'NONE',  ( 1.000000000000000000, -3.552713678800500929E-15, 0.000000000000000000 ) ) ;
#1900 = CYLINDRICAL_SURFACE ( 'NONE', #4877, 0.5000000000000004441 ) ;
#1901 = ORIENTED_EDGE ( 'NONE', *, *, #12563, .F. ) ;
#1902 =( NAMED_UNIT ( * ) PLANE_ANGLE_UNIT ( ) SI_UNIT ( $, .RADIAN. ) );
#1903 = CARTESIAN_POINT ( 'NONE',  ( 48.29629131445336299, 12.94095225512624303, 8.000000000000000000 ) ) ;
#1904 = ORIENTED_EDGE ( 'NONE', *, *, #7578, .F. ) ;
#1905 = CARTESIAN_POINT ( 'NONE',  ( 47.00000000000001421, 81.24038404635960831, 16.00000000000000000 ) ) ;
#1906 = VERTEX_POINT ( 'NONE', #8917 ) ;
#1907 = EDGE_LOOP ( 'NONE', ( #14747, #12378, #1018, #1761 ) ) ;
#1908 = DIRECTION ( 'NONE',  ( -0.000000000000000000, -0.000000000000000000, -1.000000000000000000 ) ) ;
#1909 = CARTESIAN_POINT ( 'NONE',  ( -4.211140560182194292, 2.431303136016534250, -3.745885042887433958 ) ) ;
#1910 = CARTESIAN_POINT ( 'NONE',  ( 51.79945067148123883, 13.60620885621592002, -10.50000000000000000 ) ) ;
#1911 = FACE_OUTER_BOUND ( 'NONE', #12810, .T. ) ;
#1912 = EDGE_CURVE ( 'NONE', #6451, #11873, #1123, .T. ) ;
#1913 = LINE ( 'NONE', #5419, #1312 ) ;
#1914 = VECTOR ( 'NONE', #14060, 1000.000000000000000 ) ;
#1915 = FACE_OUTER_BOUND ( 'NONE', #7710, .T. ) ;
#1916 = ORIENTED_EDGE ( 'NONE', *, *, #11920, .F. ) ;
#1917 = FACE_OUTER_BOUND ( 'NONE', #5552, .T. ) ;
#1918 = DIRECTION ( 'NONE',  ( -1.000000000000000000, 0.000000000000000000, 0.000000000000000000 ) ) ;
#1919 = CARTESIAN_POINT ( 'NONE',  ( 90.11631465359491244, 37.12029293941346708, 10.49999999999999822 ) ) ;
#1920 = VERTEX_POINT ( 'NONE', #666 ) ;
#1921 = ORIENTED_EDGE ( 'NONE', *, *, #458, .F. ) ;
#1922 = CARTESIAN_POINT ( 'NONE',  ( -47.21331623427138879, -33.48561063518577896, 10.49999999999999822 ) ) ;
#1923 = AXIS2_PLACEMENT_3D ( 'NONE', #5073, #9687, #2647 ) ;
#1924 = VERTEX_POINT ( 'NONE', #14634 ) ;
#1925 = CARTESIAN_POINT ( 'NONE',  ( 2.649999999999988809, 38.00000000000000000, 14.49999999999999822 ) ) ;
#1926 = DIRECTION ( 'NONE',  ( 0.000000000000000000, 0.000000000000000000, 1.000000000000000000 ) ) ;
#1927 = ORIENTED_EDGE ( 'NONE', *, *, #6462, .F. ) ;
#1928 = EDGE_CURVE ( 'NONE', #4839, #11834, #12993, .T. ) ;
#1929 = DIRECTION ( 'NONE',  ( 0.000000000000000000, 0.000000000000000000, 1.000000000000000000 ) ) ;
#1930 = EDGE_CURVE ( 'NONE', #4116, #8471, #9582, .T. ) ;
#1931 = DIRECTION ( 'NONE',  ( 0.000000000000000000, 0.000000000000000000, 1.000000000000000000 ) ) ;
#1932 = ORIENTED_EDGE ( 'NONE', *, *, #3289, .T. ) ;
#1933 = CIRCLE ( 'NONE', #11654, 2.500000000000000888 ) ;
#1934 = CIRCLE ( 'NONE', #10177, 2.500000000000000444 ) ;
#1935 = VERTEX_POINT ( 'NONE', #2932 ) ;
#1936 = ORIENTED_EDGE ( 'NONE', *, *, #7601, .T. ) ;
#1937 = AXIS2_PLACEMENT_3D ( 'NONE', #14153, #9363, #9287 ) ;
#1938 = CYLINDRICAL_SURFACE ( 'NONE', #8862, 5.000000000000000888 ) ;
#1939 = AXIS2_PLACEMENT_3D ( 'NONE', #5787, #1108, #5723 ) ;
#1940 = CARTESIAN_POINT ( 'NONE',  ( -26.99988008862626643, -45.88839665196127271, -13.00000000000000178 ) ) ;
#1941 = CIRCLE ( 'NONE', #5811, 63.00000000000000000 ) ;
#1942 = DIRECTION ( 'NONE',  ( 0.000000000000000000, 0.000000000000000000, 1.000000000000000000 ) ) ;
#1943 = ORIENTED_EDGE ( 'NONE', *, *, #9597, .F. ) ;
#1944 = EDGE_CURVE ( 'NONE', #11994, #12800, #14205, .T. ) ;
#1945 = EDGE_LOOP ( 'NONE', ( #2514, #8632, #7779, #11237 ) ) ;
#1946 = EDGE_LOOP ( 'NONE', ( #6602, #8176, #12056, #2754, #6989 ) ) ;
#1947 = ORIENTED_EDGE ( 'NONE', *, *, #2820, .T. ) ;
#1948 = CIRCLE ( 'NONE', #10432, 60.50000000000000000 ) ;
#1949 = CARTESIAN_POINT ( 'NONE',  ( 38.79014761921568777, 11.74264578624841171, -28.00000000000000000 ) ) ;
#1950 = VECTOR ( 'NONE', #5524, 1000.000000000000000 ) ;
#1951 = EDGE_CURVE ( 'NONE', #1381, #2743, #6422, .T. ) ;
#1952 = AXIS2_PLACEMENT_3D ( 'NONE', #10612, #211, #11772 ) ;
#1953 = FACE_OUTER_BOUND ( 'NONE', #6368, .T. ) ;
#1954 =( NAMED_UNIT ( * ) SI_UNIT ( $, .STERADIAN. ) SOLID_ANGLE_UNIT ( ) );
#1955 = CARTESIAN_POINT ( 'NONE',  ( 18.00000000000000355, 0.000000000000000000, -45.50000000000000000 ) ) ;
#1956 = EDGE_LOOP ( 'NONE', ( #7658, #2818, #11568, #9147, #13939, #884 ) ) ;
#1957 = DIRECTION ( 'NONE',  ( -0.000000000000000000, -0.000000000000000000, 1.000000000000000000 ) ) ;
#1958 = CARTESIAN_POINT ( 'NONE',  ( -12.39897948556635754, 61.76783392443436327, -16.00000000000000000 ) ) ;
#1959 = ORIENTED_EDGE ( 'NONE', *, *, #1746, .T. ) ;
#1960 = CIRCLE ( 'NONE', #9699, 59.50000000000000000 ) ;
#1961 = CARTESIAN_POINT ( 'NONE',  ( 97.50000000000000000, -3.384287605079545030E-13, -10.50000000000000000 ) ) ;
#1962 = EDGE_LOOP ( 'NONE', ( #4881, #11336, #10308, #6264, #3877, #3089 ) ) ;
#1963 = CIRCLE ( 'NONE', #12393, 60.50000000000000000 ) ;
#1964 = AXIS2_PLACEMENT_3D ( 'NONE', #10770, #4019, #9764 ) ;
#1965 = ORIENTED_EDGE ( 'NONE', *, *, #11367, .F. ) ;
#1966 = CYLINDRICAL_SURFACE ( 'NONE', #11306, 3.000000000000002665 ) ;
#1967 = PLANE ( 'NONE',  #8496 ) ;
#1968 = VECTOR ( 'NONE', #6575, 1000.000000000000000 ) ;
#1969 = FACE_OUTER_BOUND ( 'NONE', #837, .T. ) ;
#1970 = DIRECTION ( 'NONE',  ( 1.000000000000000000, 0.000000000000000000, 0.000000000000000000 ) ) ;
#1971 = CARTESIAN_POINT ( 'NONE',  ( -14.07862063237857342, 50.84834283437004387, 10.49999999999999822 ) ) ;
#1972 = CIRCLE ( 'NONE', #5846, 60.50000000000000000 ) ;
#1973 = ORIENTED_EDGE ( 'NONE', *, *, #14260, .T. ) ;
#1974 = CARTESIAN_POINT ( 'NONE',  ( 0.000000000000000000, 0.000000000000000000, 0.000000000000000000 ) ) ;
#1975 = PRODUCT_DEFINITION_SHAPE ( 'NONE', 'NONE',  #15042 ) ;
#1976 = ADVANCED_FACE ( 'NONE', ( #14550 ), #14777, .F. ) ;
#1977 = DIRECTION ( 'NONE',  ( -1.000000000000000000, 0.000000000000000000, 0.000000000000000000 ) ) ;
#1978 = CARTESIAN_POINT ( 'NONE',  ( 13.71740939043365337, -51.19406879332061067, -13.00000000000000178 ) ) ;
#1979 = EDGE_CURVE ( 'NONE', #6594, #3549, #6409, .T. ) ;
#1980 = AXIS2_PLACEMENT_3D ( 'NONE', #11041, #3623, #8747 ) ;
#1981 = VERTEX_POINT ( 'NONE', #11293 ) ;
#1982 = DIRECTION ( 'NONE',  ( 0.000000000000000000, 0.000000000000000000, -1.000000000000000000 ) ) ;
#1983 = ORIENTED_EDGE ( 'NONE', *, *, #2278, .T. ) ;
#1984 = DIRECTION ( 'NONE',  ( 0.000000000000000000, 0.000000000000000000, 1.000000000000000000 ) ) ;
#1985 = AXIS2_PLACEMENT_3D ( 'NONE', #8037, #13580, #11320 ) ;
#1986 = ORIENTED_EDGE ( 'NONE', *, *, #7871, .F. ) ;
#1987 = CARTESIAN_POINT ( 'NONE',  ( 0.000000000000000000, 0.000000000000000000, -10.50000000000000000 ) ) ;
#1988 = EDGE_CURVE ( 'NONE', #8172, #5421, #5442, .T. ) ;
#1989 = ORIENTED_EDGE ( 'NONE', *, *, #11600, .T. ) ;
#1990 = DIRECTION ( 'NONE',  ( -1.000000000000000000, 0.000000000000000000, 0.000000000000000000 ) ) ;
#1991 = DIRECTION ( 'NONE',  ( 0.000000000000000000, 0.000000000000000000, 1.000000000000000000 ) ) ;
#1992 = DIRECTION ( 'NONE',  ( 1.000000000000000000, 0.000000000000000000, 0.000000000000000000 ) ) ;
#1993 = DIRECTION ( 'NONE',  ( 1.000000000000000000, 0.000000000000000000, 0.000000000000000000 ) ) ;
#1994 = CYLINDRICAL_SURFACE ( 'NONE', #13203, 0.5000000000000038858 ) ;
#1995 = ADVANCED_FACE ( 'NONE', ( #896 ), #4080, .T. ) ;
#1996 = ORIENTED_EDGE ( 'NONE', *, *, #8322, .T. ) ;
#1997 = CIRCLE ( 'NONE', #1046, 3.000000000000002665 ) ;
#1998 = ADVANCED_FACE ( 'NONE', ( #7635 ), #12201, .T. ) ;
#1999 = DIRECTION ( 'NONE',  ( 0.000000000000000000, 0.000000000000000000, 1.000000000000000000 ) ) ;
#2000 = CARTESIAN_POINT ( 'NONE',  ( 11.63111172283970518, 94.28541358805125583, -17.83102282485378254 ) ) ;
#2001 = DIRECTION ( 'NONE',  ( 1.000000000000000000, 0.000000000000000000, 0.000000000000000000 ) ) ;
#2002 = DIRECTION ( 'NONE',  ( -1.000000000000000000, 0.000000000000000000, 0.000000000000000000 ) ) ;
#2003 = CIRCLE ( 'NONE', #14123, 63.00000000000000000 ) ;
#2004 = ORIENTED_EDGE ( 'NONE', *, *, #1008, .T. ) ;
#2005 = CARTESIAN_POINT ( 'NONE',  ( 68.68541276968825571, -69.08004447556089644, -13.00000000000000178 ) ) ;
#2006 = EDGE_LOOP ( 'NONE', ( #5820, #12503, #5156, #9195 ) ) ;
#2007 = DIRECTION ( 'NONE',  ( 0.000000000000000000, 0.000000000000000000, -1.000000000000000000 ) ) ;
#2008 = LINE ( 'NONE', #14702, #12657 ) ;
#2009 = AXIS2_PLACEMENT_3D ( 'NONE', #10521, #4611, #3471 ) ;
#2010 = CARTESIAN_POINT ( 'NONE',  ( -68.08935777509570642, -68.58935777509452691, -13.00000000000000178 ) ) ;
#2011 = CARTESIAN_POINT ( 'NONE',  ( 97.00000000000000000, -3.384287605079545030E-13, -10.50000000000000000 ) ) ;
#2012 = CONTEXT_DEPENDENT_SHAPE_REPRESENTATION ( #8333, #6444 ) ;
#2013 = ORIENTED_EDGE ( 'NONE', *, *, #7396, .T. ) ;
#2014 = VERTEX_POINT ( 'NONE', #7784 ) ;
#2015 = ORIENTED_EDGE ( 'NONE', *, *, #9266, .F. ) ;
#2016 = CARTESIAN_POINT ( 'NONE',  ( -7.500000000000000888, 59.24038404635959409, 15.00000000000000000 ) ) ;
#2017 = CARTESIAN_POINT ( 'NONE',  ( 0.000000000000000000, 0.000000000000000000, -26.00000000000000000 ) ) ;
#2018 = AXIS2_PLACEMENT_3D ( 'NONE', #5999, #4885, #14142 ) ;
#2019 = DIRECTION ( 'NONE',  ( -0.9557692240748186796, 0.2941176470588241498, -1.531423350357148967E-16 ) ) ;
#2020 = ORIENTED_EDGE ( 'NONE', *, *, #3944, .T. ) ;
#2021 = EDGE_CURVE ( 'NONE', #2752, #9052, #3302, .T. ) ;
#2022 = CIRCLE ( 'NONE', #11732, 59.50000000000000000 ) ;
#2023 = EDGE_CURVE ( 'NONE', #1639, #1264, #7705, .T. ) ;
#2024 = EDGE_LOOP ( 'NONE', ( #3147, #13532, #9238, #14993, #2848, #8079, #6197, #9100, #13934, #3016, #4925, #7406 ) ) ;
#2025 = ORIENTED_EDGE ( 'NONE', *, *, #8699, .F. ) ;
#2026 = EDGE_CURVE ( 'NONE', #8852, #9388, #6577, .T. ) ;
#2027 = VECTOR ( 'NONE', #13115, 1000.000000000000000 ) ;
#2028 = DIRECTION ( 'NONE',  ( 0.000000000000000000, 0.000000000000000000, -1.000000000000000000 ) ) ;
#2029 = CARTESIAN_POINT ( 'NONE',  ( -68.58935777509570642, -68.58935777509452691, 10.49999999999999822 ) ) ;
#2030 = DIRECTION ( 'NONE',  ( 0.000000000000000000, 0.000000000000000000, -1.000000000000000000 ) ) ;
#2031 = CARTESIAN_POINT ( 'NONE',  ( 34.44830544488820578, 94.94374256356071839, -16.00000000000000000 ) ) ;
#2032 = ADVANCED_FACE ( 'NONE', ( #12122 ), #1938, .F. ) ;
#2033 = AXIS2_PLACEMENT_3D ( 'NONE', #8078, #6932, #32 ) ;
#2034 = ORIENTED_EDGE ( 'NONE', *, *, #8597, .F. ) ;
#2035 = LINE ( 'NONE', #753, #1481 ) ;
#2036 = CARTESIAN_POINT ( 'NONE',  ( -31.59365702568382872, 102.2290646705776140, 12.13969626787233480 ) ) ;
#2037 = ORIENTED_EDGE ( 'NONE', *, *, #4269, .F. ) ;
#2038 = DIRECTION ( 'NONE',  ( -0.000000000000000000, -0.000000000000000000, 1.000000000000000000 ) ) ;
#2039 = EDGE_LOOP ( 'NONE', ( #6393, #1428, #10649, #1916 ) ) ;
#2040 = EDGE_CURVE ( 'NONE', #11760, #11078, #3545, .T. ) ;
#2041 = ORIENTED_EDGE ( 'NONE', *, *, #8973, .T. ) ;
#2042 = CARTESIAN_POINT ( 'NONE',  ( -7.500000000000000000, 94.70348462437907244, -20.00000000000000000 ) ) ;
#2043 = CIRCLE ( 'NONE', #5440, 63.00000000000000000 ) ;
#2044 = CIRCLE ( 'NONE', #8575, 63.00000000000000000 ) ;
#2045 = AXIS2_PLACEMENT_3D ( 'NONE', #13018, #2534, #11879 ) ;
#2046 = LINE ( 'NONE', #8939, #5832 ) ;
#2047 = DIRECTION ( 'NONE',  ( -0.000000000000000000, 0.000000000000000000, -1.000000000000000000 ) ) ;
#2048 = DIRECTION ( 'NONE',  ( 1.000000000000000000, 0.000000000000000000, 0.000000000000000000 ) ) ;
#2049 = DIRECTION ( 'NONE',  ( 0.000000000000000000, 0.000000000000000000, 1.000000000000000000 ) ) ;
#2050 = CARTESIAN_POINT ( 'NONE',  ( 0.000000000000000000, 0.000000000000000000, -8.000000000000000000 ) ) ;
#2051 = VERTEX_POINT ( 'NONE', #13947 ) ;
#2052 = CIRCLE ( 'NONE', #8828, 2.041999999999999815 ) ;
#2053 = VECTOR ( 'NONE', #14016, 1000.000000000000000 ) ;
#2054 = PLANE ( 'NONE',  #11174 ) ;
#2055 = AXIS2_PLACEMENT_3D ( 'NONE', #9914, #7711, #13494 ) ;
#2056 = CARTESIAN_POINT ( 'NONE',  ( 9.717538815323484513, 62.24844358264333266, 19.51802576651051879 ) ) ;
#2057 = DIRECTION ( 'NONE',  ( 0.000000000000000000, 0.000000000000000000, 1.000000000000000000 ) ) ;
#2058 = B_SPLINE_CURVE_WITH_KNOTS ( 'NONE', 3,
 ( #11031, #11871, #10801, #550, #4966, #9642 ),
 .UNSPECIFIED., .F., .F.,
 ( 4, 2, 4 ),
 ( 0.002452478801916362864, 0.003676905084148002212, 0.004901331366379641993 ),
 .UNSPECIFIED. ) ;
#2059 = ORIENTED_EDGE ( 'NONE', *, *, #451, .T. ) ;
#2060 = FACE_OUTER_BOUND ( 'NONE', #12721, .T. ) ;
#2061 = AXIS2_PLACEMENT_3D ( 'NONE', #6290, #9869, #13451 ) ;
#2062 = CARTESIAN_POINT ( 'NONE',  ( 0.000000000000000000, 0.000000000000000000, -23.50000000000000000 ) ) ;
#2063 = ORIENTED_EDGE ( 'NONE', *, *, #13768, .F. ) ;
#2064 = CIRCLE ( 'NONE', #6658, 5.560781378645573980 ) ;
#2065 = CIRCLE ( 'NONE', #2767, 95.00000000000001421 ) ;
#2066 = DIRECTION ( 'NONE',  ( 0.000000000000000000, 0.000000000000000000, 1.000000000000000000 ) ) ;
#2067 = CARTESIAN_POINT ( 'NONE',  ( -45.83364790889027773, 29.49928053175948506, -8.000000000000000000 ) ) ;
#2068 = DIRECTION ( 'NONE',  ( 0.000000000000000000, 0.000000000000000000, 1.000000000000000000 ) ) ;
#2069 = ADVANCED_FACE ( 'NONE', ( #10363 ), #4672, .T. ) ;
#2070 = DIRECTION ( 'NONE',  ( 1.000000000000000000, 0.000000000000000000, 0.000000000000000000 ) ) ;
#2071 = DIRECTION ( 'NONE',  ( -0.000000000000000000, -0.000000000000000000, -1.000000000000000000 ) ) ;
#2072 = CARTESIAN_POINT ( 'NONE',  ( -29.70588235294118107, 96.53269163155674448, 10.99999999999999645 ) ) ;
#2073 = AXIS2_PLACEMENT_3D ( 'NONE', #14423, #4027, #8641 ) ;
#2074 = ORIENTED_EDGE ( 'NONE', *, *, #9353, .F. ) ;
#2075 = DIRECTION ( 'NONE',  ( 1.000000000000000000, 0.000000000000000000, 0.000000000000000000 ) ) ;
#2076 = CARTESIAN_POINT ( 'NONE',  ( 12.39897948556635754, 100.2360479454198696, -16.00000000000000000 ) ) ;
#2077 = CIRCLE ( 'NONE', #14932, 2.500000000000000444 ) ;
#2078 = CARTESIAN_POINT ( 'NONE',  ( 5.200000000000006395, 0.000000000000000000, 2.775557561562891351E-14 ) ) ;
#2079 = B_SPLINE_CURVE_WITH_KNOTS ( 'NONE', 3,
 ( #12833, #8352, #11852, #7273, #3808, #2503 ),
 .UNSPECIFIED., .F., .F.,
 ( 4, 2, 4 ),
 ( 0.003358874760055550589, 0.004541967308452098118, 0.005725059856848646080 ),
 .UNSPECIFIED. ) ;
#2080 = DIRECTION ( 'NONE',  ( 1.000000000000000000, 0.000000000000000000, 0.000000000000000000 ) ) ;
#2081 = ORIENTED_EDGE ( 'NONE', *, *, #9552, .F. ) ;
#2082 = VECTOR ( 'NONE', #11899, 1000.000000000000000 ) ;
#2083 = CARTESIAN_POINT ( 'NONE',  ( 0.1410422978106151692, -4.700232962125109104, -3.687027686973631369 ) ) ;
#2084 = CIRCLE ( 'NONE', #10569, 57.00000000000000000 ) ;
#2085 = VERTEX_POINT ( 'NONE', #14935 ) ;
#2086 = DIRECTION ( 'NONE',  ( 0.000000000000000000, 0.000000000000000000, 1.000000000000000000 ) ) ;
#2087 = ADVANCED_FACE ( 'NONE', ( #12724 ), #10291, .F. ) ;
#2088 = DIRECTION ( 'NONE',  ( -0.000000000000000000, -0.000000000000000000, 1.000000000000000000 ) ) ;
#2089 = EDGE_CURVE ( 'NONE', #11234, #5062, #7461, .T. ) ;
#2090 = VERTEX_POINT ( 'NONE', #6937 ) ;
#2091 = CARTESIAN_POINT ( 'NONE',  ( 12.50000000000000178, 106.2673515243511275, -15.33085973118640055 ) ) ;
#2092 = DIRECTION ( 'NONE',  ( -1.000000000000000000, 0.000000000000000000, 0.000000000000000000 ) ) ;
#2093 = PRODUCT_CONTEXT ( 'NONE', #7647, 'mechanical' ) ;
#2094 = VERTEX_POINT ( 'NONE', #6777 ) ;
#2095 = EDGE_CURVE ( 'NONE', #3662, #6497, #13746, .T. ) ;
#2096 = ORIENTED_EDGE ( 'NONE', *, *, #9708, .T. ) ;
#2097 = CARTESIAN_POINT ( 'NONE',  ( -10.21169758550232309, 62.16852661215632025, -19.23993411931846609 ) ) ;
#2098 = CARTESIAN_POINT ( 'NONE',  ( 32.65306121041741960, 101.8676703390407283, 14.32076206672372365 ) ) ;
#2099 = CARTESIAN_POINT ( 'NONE',  ( -3.492805317593278058, 46.55633131742322917, -10.50000000000000000 ) ) ;
#2100 = ORIENTED_EDGE ( 'NONE', *, *, #8157, .T. ) ;
#2101 = ORIENTED_EDGE ( 'NONE', *, *, #11960, .F. ) ;
#2102 = EDGE_LOOP ( 'NONE', ( #6144, #14266, #378, #1064 ) ) ;
#2103 = CIRCLE ( 'NONE', #2833, 3.000000000000002665 ) ;
#2104 = DIRECTION ( 'NONE',  ( 0.000000000000000000, 0.000000000000000000, -1.000000000000000000 ) ) ;
#2105 = CARTESIAN_POINT ( 'NONE',  ( -13.71740939043329277, 51.19406879332069593, -10.50000000000000000 ) ) ;
#2106 = DIRECTION ( 'NONE',  ( -1.000000000000000000, 0.000000000000000000, 0.000000000000000000 ) ) ;
#2107 = DIRECTION ( 'NONE',  ( 0.000000000000000000, 0.000000000000000000, -1.000000000000000000 ) ) ;
#2108 = ORIENTED_EDGE ( 'NONE', *, *, #2903, .F. ) ;
#2109 = FACE_BOUND ( 'NONE', #8563, .T. ) ;
#2110 = DIRECTION ( 'NONE',  ( 1.000000000000000000, 0.000000000000000000, -0.000000000000000000 ) ) ;
#2111 = EDGE_CURVE ( 'NONE', #13137, #13279, #6687, .T. ) ;
#2112 = ORIENTED_EDGE ( 'NONE', *, *, #6887, .F. ) ;
#2113 = CARTESIAN_POINT ( 'NONE',  ( -31.74999999999995737, 0.000000000000000000, -2.775557561562891351E-14 ) ) ;
#2114 = EDGE_CURVE ( 'NONE', #1981, #7885, #154, .T. ) ;
#2115 = EDGE_LOOP ( 'NONE', ( #13214, #3973, #6177, #9245 ) ) ;
#2116 = ORIENTED_EDGE ( 'NONE', *, *, #12114, .F. ) ;
#2117 = DIRECTION ( 'NONE',  ( 0.000000000000000000, -0.000000000000000000, 1.000000000000000000 ) ) ;
#2118 = EDGE_CURVE ( 'NONE', #11737, #13523, #5959, .T. ) ;
#2119 = VERTEX_POINT ( 'NONE', #11665 ) ;
#2120 = DIRECTION ( 'NONE',  ( 0.000000000000000000, 0.000000000000000000, 1.000000000000000000 ) ) ;
#2121 = CARTESIAN_POINT ( 'NONE',  ( -22.05882352941176450, 71.68269180561142662, -23.50000000000000000 ) ) ;
#2122 = DIRECTION ( 'NONE',  ( 0.000000000000000000, 0.000000000000000000, 1.000000000000000000 ) ) ;
#2123 = DIRECTION ( 'NONE',  ( 0.000000000000000000, 0.000000000000000000, 1.000000000000000000 ) ) ;
#2124 = EDGE_CURVE ( 'NONE', #8389, #4446, #14462, .T. ) ;
#2125 = DIRECTION ( 'NONE',  ( -0.000000000000000000, -0.000000000000000000, 1.000000000000000000 ) ) ;
#2126 = EDGE_CURVE ( 'NONE', #12800, #12895, #4766, .T. ) ;
#2127 = ORIENTED_EDGE ( 'NONE', *, *, #5878, .F. ) ;
#2128 = FACE_BOUND ( 'NONE', #5019, .T. ) ;
#2129 = DIRECTION ( 'NONE',  ( -0.000000000000000000, -0.000000000000000000, 1.000000000000000000 ) ) ;
#2130 = CARTESIAN_POINT ( 'NONE',  ( -4.204015924366186319, 1.626724848190920891, -3.610627190413389975 ) ) ;
#2131 = ORIENTED_EDGE ( 'NONE', *, *, #9963, .F. ) ;
#2132 = CARTESIAN_POINT ( 'NONE',  ( -4.197393957002300446, -0.8151795401431412014, -3.503767560748934251 ) ) ;
#2133 = ADVANCED_FACE ( 'NONE', ( #12504 ), #7908, .T. ) ;
#2134 = DIRECTION ( 'NONE',  ( 0.000000000000000000, 0.000000000000000000, 1.000000000000000000 ) ) ;
#2135 = AXIS2_PLACEMENT_3D ( 'NONE', #8102, #2337, #12815 ) ;
#2136 = CARTESIAN_POINT ( 'NONE',  ( 45.83364790889049090, -29.49928053175916887, -13.00000000000000178 ) ) ;
#2137 = DIRECTION ( 'NONE',  ( -1.000000000000000000, 0.000000000000000000, 0.000000000000000000 ) ) ;
#2138 = CARTESIAN_POINT ( 'NONE',  ( -12.46747951117848885, 106.2711918341631900, 15.65812229356676433 ) ) ;
#2139 = CARTESIAN_POINT ( 'NONE',  ( -31.74999999999995737, 0.000000000000000000, 2.499999999999972911 ) ) ;
#2140 = DIRECTION ( 'NONE',  ( -1.000000000000000000, 0.000000000000000000, 0.000000000000000000 ) ) ;
#2141 = CARTESIAN_POINT ( 'NONE',  ( 0.000000000000000000, 0.000000000000000000, -4.000000000000000000 ) ) ;
#2142 = ORIENTED_EDGE ( 'NONE', *, *, #7165, .F. ) ;
#2143 = CARTESIAN_POINT ( 'NONE',  ( 0.000000000000000000, 0.000000000000000000, 8.000000000000000000 ) ) ;
#2144 = VERTEX_POINT ( 'NONE', #8161 ) ;
#2145 = CARTESIAN_POINT ( 'NONE',  ( 25.00000000000000000, 81.24038404635960831, -26.00000000000000000 ) ) ;
#2146 = DIRECTION ( 'NONE',  ( 1.000000000000000000, 0.000000000000000000, 0.000000000000000000 ) ) ;
#2147 = DIRECTION ( 'NONE',  ( 0.000000000000000000, 0.000000000000000000, -1.000000000000000000 ) ) ;
#2148 = DIRECTION ( 'NONE',  ( 0.000000000000000000, 0.000000000000000000, 1.000000000000000000 ) ) ;
#2149 = VERTEX_POINT ( 'NONE', #4458 ) ;
#2150 = CARTESIAN_POINT ( 'NONE',  ( 39.30189486418243661, 33.47282819776626894, -8.000000000000000000 ) ) ;
#2151 = ORIENTED_EDGE ( 'NONE', *, *, #10847, .F. ) ;
#2152 = CARTESIAN_POINT ( 'NONE',  ( 42.04772703543530099, 32.26435573746242369, 8.000000000000000000 ) ) ;
#2153 = PRESENTATION_STYLE_ASSIGNMENT (( #6769 ) ) ;
#2154 = CARTESIAN_POINT ( 'NONE',  ( 39.61975340586557337, 91.27544013909754028, -8.000000000000000000 ) ) ;
#2155 = DIRECTION ( 'NONE',  ( 0.000000000000000000, 0.000000000000000000, 1.000000000000000000 ) ) ;
#2156 = ORIENTED_EDGE ( 'NONE', *, *, #5373, .F. ) ;
#2157 = ORIENTED_EDGE ( 'NONE', *, *, #4361, .F. ) ;
#2158 = ORIENTED_EDGE ( 'NONE', *, *, #8886, .T. ) ;
#2159 = EDGE_CURVE ( 'NONE', #8152, #4787, #8872, .T. ) ;
#2160 = CARTESIAN_POINT ( 'NONE',  ( -8.635061085254617907, 62.40781208424768778, -19.90323072647615987 ) ) ;
#2161 = CARTESIAN_POINT ( 'NONE',  ( 7.500000000000000000, 94.70348462437907244, 20.00000000000000000 ) ) ;
#2162 = EDGE_CURVE ( 'NONE', #14615, #10761, #10089, .T. ) ;
#2163 = FACE_OUTER_BOUND ( 'NONE', #14405, .T. ) ;
#2164 = ADVANCED_FACE ( 'NONE', ( #11527 ), #3315, .F. ) ;
#2166 = EDGE_LOOP ( 'NONE', ( #3676, #4232, #10209, #586 ) ) ;
#2165 = EDGE_CURVE ( 'NONE', #697, #11955, #4599, .T. ) ;
#2167 = AXIS2_PLACEMENT_3D ( 'NONE', #8647, #6281, #13288 ) ;
#2168 = ORIENTED_EDGE ( 'NONE', *, *, #14901, .T. ) ;
#2169 = ORIENTED_EDGE ( 'NONE', *, *, #12047, .T. ) ;
#2170 = CARTESIAN_POINT ( 'NONE',  ( 9.706343076449424956, 74.36968214894433515, 19.49591231693629112 ) ) ;
#2171 = VECTOR ( 'NONE', #12032, 1000.000000000000000 ) ;
#2172 = DIRECTION ( 'NONE',  ( -1.000000000000000000, 0.000000000000000000, 0.000000000000000000 ) ) ;
#2173 = DIRECTION ( 'NONE',  ( 0.000000000000000000, 0.000000000000000000, 1.000000000000000000 ) ) ;
#2174 = CARTESIAN_POINT ( 'NONE',  ( 0.000000000000000000, 0.000000000000000000, -8.000000000000000000 ) ) ;
#2175 = ORIENTED_EDGE ( 'NONE', *, *, #11477, .F. ) ;
#2176 = CARTESIAN_POINT ( 'NONE',  ( -26.49999999999971578, -45.89934640057541060, 8.000000000000000000 ) ) ;
#2177 = EDGE_LOOP ( 'NONE', ( #8294, #8233 ) ) ;
#2178 = CIRCLE ( 'NONE', #5335, 3.000000000000002665 ) ;
#2179 = EDGE_CURVE ( 'NONE', #2876, #12336, #12046, .T. ) ;
#2180 = CARTESIAN_POINT ( 'NONE',  ( 12.50000000000000000, 100.2235002382176248, -79.80561291909842225 ) ) ;
#2181 = DIRECTION ( 'NONE',  ( 0.000000000000000000, 0.000000000000000000, -1.000000000000000000 ) ) ;
#2182 = EDGE_CURVE ( 'NONE', #10943, #3127, #9122, .T. ) ;
#2183 = ORIENTED_EDGE ( 'NONE', *, *, #4231, .T. ) ;
#2184 = PRODUCT_DEFINITION_FORMATION_WITH_SPECIFIED_SOURCE ( 'ANY', '', #11452, .NOT_KNOWN. ) ;
#2185 = VECTOR ( 'NONE', #703, 1000.000000000000000 ) ;
#2186 = EDGE_LOOP ( 'NONE', ( #3065, #6709, #2536, #9817, #10492, #1577, #4627, #4554, #8167, #12707, #634 ) ) ;
#2187 = DIRECTION ( 'NONE',  ( 1.000000000000000000, 0.000000000000000000, 0.000000000000000000 ) ) ;
#2188 = AXIS2_PLACEMENT_3D ( 'NONE', #3211, #941, #14687 ) ;
#2189 = AXIS2_PLACEMENT_3D ( 'NONE', #11339, #6458, #1771 ) ;
#2190 = ORIENTED_EDGE ( 'NONE', *, *, #9392, .T. ) ;
#2191 = EDGE_LOOP ( 'NONE', ( #4825, #12319 ) ) ;
#2192 = DIRECTION ( 'NONE',  ( 0.000000000000000000, -1.000000000000000000, 0.000000000000000000 ) ) ;
#2193 = DIRECTION ( 'NONE',  ( -1.000000000000000000, 0.000000000000000000, 0.000000000000000000 ) ) ;
#2194 = DIRECTION ( 'NONE',  ( 0.000000000000000000, 0.000000000000000000, 1.000000000000000000 ) ) ;
#2195 = DIRECTION ( 'NONE',  ( 1.000000000000000000, 0.000000000000000000, 0.000000000000000000 ) ) ;
#2196 = CIRCLE ( 'NONE', #7312, 2.700000000000000622 ) ;
#2197 = AXIS2_PLACEMENT_3D ( 'NONE', #6730, #12898, #10320 ) ;
#2198 = CARTESIAN_POINT ( 'NONE',  ( -25.00000000000000000, 81.24038404635962252, -16.00000000000000000 ) ) ;
#2199 = ORIENTED_EDGE ( 'NONE', *, *, #6005, .T. ) ;
#2200 = CIRCLE ( 'NONE', #3171, 59.49999999999999289 ) ;
#2201 = DIRECTION ( 'NONE',  ( -0.000000000000000000, -0.000000000000000000, -1.000000000000000000 ) ) ;
#2202 = CIRCLE ( 'NONE', #11426, 53.55662432702593634 ) ;
#2203 = CIRCLE ( 'NONE', #10685, 2.100000000000000089 ) ;
#2204 = CARTESIAN_POINT ( 'NONE',  ( -22.33583958711380646, -30.74264578624812927, -25.50000000000000355 ) ) ;
#2205 = CARTESIAN_POINT ( 'NONE',  ( -13.71740939043329277, 51.19406879332069593, -8.000000000000000000 ) ) ;
#2206 = ORIENTED_EDGE ( 'NONE', *, *, #8195, .T. ) ;
#2207 = CYLINDRICAL_SURFACE ( 'NONE', #5469, 63.00000000000000000 ) ;
#2208 = CIRCLE ( 'NONE', #14821, 2.649999999999992806 ) ;
#2209 = ORIENTED_EDGE ( 'NONE', *, *, #4162, .T. ) ;
#2210 = EDGE_CURVE ( 'NONE', #5057, #14819, #14015, .T. ) ;
#2211 = AXIS2_PLACEMENT_3D ( 'NONE', #3555, #5596, #2334 ) ;
#2212 = LINE ( 'NONE', #5550, #8334 ) ;
#2213 = ADVANCED_FACE ( 'NONE', ( #6237 ), #260, .F. ) ;
#2214 = ADVANCED_BREP_SHAPE_REPRESENTATION ( '', ( #14006, #5108 ), #3871 ) ;
#2215 = DIRECTION ( 'NONE',  ( 1.000000000000000000, 0.000000000000000000, 0.000000000000000000 ) ) ;
#2216 = AXIS2_PLACEMENT_3D ( 'NONE', #12738, #2329, #1414 ) ;
#2217 = EDGE_CURVE ( 'NONE', #3842, #3184, #11317, .T. ) ;
#2218 = ADVANCED_FACE ( 'NONE', ( #5043 ), #7228, .T. ) ;
#2219 = VECTOR ( 'NONE', #3531, 999.9999999999998863 ) ;
#2220 = CYLINDRICAL_SURFACE ( 'NONE', #14187, 0.5000000000000073275 ) ;
#2221 = CARTESIAN_POINT ( 'NONE',  ( 13.58799986788239345, -50.71110588017607768, -10.50000000000000000 ) ) ;
#2222 = CARTESIAN_POINT ( 'NONE',  ( 0.000000000000000000, 0.000000000000000000, 13.50000000000000533 ) ) ;
#2223 = DIRECTION ( 'NONE',  ( 0.000000000000000000, 0.000000000000000000, -1.000000000000000000 ) ) ;
#2224 = EDGE_CURVE ( 'NONE', #13003, #10670, #5007, .T. ) ;
#2225 = CARTESIAN_POINT ( 'NONE',  ( 37.12029293941379393, 89.61631465359479876, -8.000000000000000000 ) ) ;
#2226 = AXIS2_PLACEMENT_3D ( 'NONE', #11378, #50, #1136 ) ;
#2227 = ORIENTED_EDGE ( 'NONE', *, *, #9425, .T. ) ;
#2228 = DIRECTION ( 'NONE',  ( 0.000000000000000000, 0.000000000000000000, -1.000000000000000000 ) ) ;
#2229 = CARTESIAN_POINT ( 'NONE',  ( 37.12029293941315444, -89.61631465359504034, -10.50000000000000000 ) ) ;
#2230 = CIRCLE ( 'NONE', #11206, 56.99999999999999289 ) ;
#2231 = DIRECTION ( 'NONE',  ( 0.000000000000000000, 0.000000000000000000, 1.000000000000000000 ) ) ;
#2232 = DIRECTION ( 'NONE',  ( 1.000000000000000000, 0.000000000000000000, 0.000000000000000000 ) ) ;
#2233 = EDGE_CURVE ( 'NONE', #10670, #13141, #4288, .T. ) ;
#2234 = ORIENTED_EDGE ( 'NONE', *, *, #12386, .T. ) ;
#2235 = CARTESIAN_POINT ( 'NONE',  ( -12.50000000000000000, 106.2673515243510991, -31.00000000000000000 ) ) ;
#2236 = ORIENTED_EDGE ( 'NONE', *, *, #14652, .F. ) ;
#2237 = AXIS2_PLACEMENT_3D ( 'NONE', #10412, #12699, #10344 ) ;
#2238 = PLANE ( 'NONE',  #10183 ) ;
#2239 = PLANE ( 'NONE',  #4437 ) ;
#2240 = DIRECTION ( 'NONE',  ( 0.000000000000000000, -0.4999999999999997780, 0.8660254037844388186 ) ) ;
#2241 =( GEOMETRIC_REPRESENTATION_CONTEXT ( 3 ) GLOBAL_UNCERTAINTY_ASSIGNED_CONTEXT ( ( #10015 ) ) GLOBAL_UNIT_ASSIGNED_CONTEXT ( ( #7698, #14926, #4667 ) ) REPRESENTATION_CONTEXT ( 'NONE', 'WORKASPACE' ) );
#2242 = DIRECTION ( 'NONE',  ( 0.000000000000000000, 0.000000000000000000, -1.000000000000000000 ) ) ;
#2243 = EDGE_LOOP ( 'NONE', ( #1298, #12351, #3364, #10250, #9546 ) ) ;
#2244 = EDGE_LOOP ( 'NONE', ( #9568, #3382, #5426, #11140 ) ) ;
#2245 = ORIENTED_EDGE ( 'NONE', *, *, #10151, .F. ) ;
#2246 = CARTESIAN_POINT ( 'NONE',  ( -52.54657765281192638, 6.917888187662934563, -10.50000000000000000 ) ) ;
#2247 = DIRECTION ( 'NONE',  ( -1.000000000000000000, 0.000000000000000000, 0.000000000000000000 ) ) ;
#2248 = AXIS2_PLACEMENT_3D ( 'NONE', #2322, #13795, #7082 ) ;
#2249 = CARTESIAN_POINT ( 'NONE',  ( -3.999999999999997335, -1.942223658245637807, -0.3516579909967631479 ) ) ;
#2250 = ORIENTED_EDGE ( 'NONE', *, *, #3584, .T. ) ;
#2251 = EDGE_LOOP ( 'NONE', ( #8830, #6113, #2806, #12169, #4823 ) ) ;
#2252 = EDGE_LOOP ( 'NONE', ( #8931, #3560, #14048, #14172, #2312 ) ) ;
#2253 = LINE ( 'NONE', #5881, #12726 ) ;
#2254 = AXIS2_PLACEMENT_3D ( 'NONE', #8603, #12949, #11816 ) ;
#2255 = CARTESIAN_POINT ( 'NONE',  ( 47.63108361037843252, 56.43380494353993271, -13.00000000000000178 ) ) ;
#2256 = CARTESIAN_POINT ( 'NONE',  ( -6.526309611002563571, -49.57224306869052555, 8.000000000000000000 ) ) ;
#2257 =( NAMED_UNIT ( * ) PLANE_ANGLE_UNIT ( ) SI_UNIT ( $, .RADIAN. ) );
#2258 = EDGE_CURVE ( 'NONE', #7227, #1401, #3554, .T. ) ;
#2259 = DIRECTION ( 'NONE',  ( 0.000000000000000000, -1.000000000000000000, 0.000000000000000000 ) ) ;
#2260 = EDGE_CURVE ( 'NONE', #5532, #9310, #3069, .T. ) ;
#2261 = ORIENTED_EDGE ( 'NONE', *, *, #8888, .T. ) ;
#2262 = DIRECTION ( 'NONE',  ( -1.000000000000000000, 7.988474494414204077E-14, 0.000000000000000000 ) ) ;
#2263 = AXIS2_PLACEMENT_3D ( 'NONE', #3445, #1237, #3522 ) ;
#2264 = VERTEX_POINT ( 'NONE', #14079 ) ;
#2265 = DIRECTION ( 'NONE',  ( 0.000000000000000000, 0.000000000000000000, 1.000000000000000000 ) ) ;
#2266 = DIRECTION ( 'NONE',  ( 1.000000000000000000, 0.000000000000000000, 0.000000000000000000 ) ) ;
#2267 = CIRCLE ( 'NONE', #10987, 60.50000000000000000 ) ;
#2268 = ORIENTED_EDGE ( 'NONE', *, *, #8857, .T. ) ;
#2269 = AXIS2_PLACEMENT_3D ( 'NONE', #6255, #9750, #1649 ) ;
#2270 = ORIENTED_EDGE ( 'NONE', *, *, #6263, .F. ) ;
#2271 = CARTESIAN_POINT ( 'NONE',  ( -89.61631465359441506, 37.12029293941468211, -8.000000000000000000 ) ) ;
#2272 = EDGE_CURVE ( 'NONE', #10943, #8733, #2540, .T. ) ;
#2273 = ORIENTED_EDGE ( 'NONE', *, *, #2763, .F. ) ;
#2274 = DIRECTION ( 'NONE',  ( 0.000000000000000000, 0.000000000000000000, 1.000000000000000000 ) ) ;
#2275 = FACE_OUTER_BOUND ( 'NONE', #2244, .T. ) ;
#2276 = CIRCLE ( 'NONE', #5174, 20.00000000000000000 ) ;
#2277 = CARTESIAN_POINT ( 'NONE',  ( -36.08010649850015028, 100.2464683348682684, 16.00000000000000000 ) ) ;
#2278 = EDGE_CURVE ( 'NONE', #4906, #12796, #11062, .T. ) ;
#2279 = B_SPLINE_CURVE_WITH_KNOTS ( 'NONE', 3,
 ( #4722, #3351, #3280, #13835, #13988, #6974, #3582, #3508, #8200, #8129, #933, #11631, #13916, #12771, #4569, #2288, #10174, #12692, #13680, #9117 ),
 .UNSPECIFIED., .F., .F.,
 ( 4, 2, 2, 2, 2, 2, 2, 2, 2, 4 ),
 ( 3.469446951953614189E-18, 0.0009765910691878101728, 0.001464886603781713308, 0.001953182138375616442, 0.002929773207563419243, 0.003906364276751221609, 0.004882955345939024409, 0.005859546415126826342, 0.006836137484314628275, 0.007812728553502431075 ),
 .UNSPECIFIED. ) ;
#2280 = ADVANCED_FACE ( 'NONE', ( #11883 ), #8384, .F. ) ;
#2281 = DIRECTION ( 'NONE',  ( 0.000000000000000000, 0.000000000000000000, -1.000000000000000000 ) ) ;
#2282 = ORIENTED_EDGE ( 'NONE', *, *, #6282, .F. ) ;
#2283 = CARTESIAN_POINT ( 'NONE',  ( -2.649999999999994138, 38.00000000000000000, -25.50000000000000355 ) ) ;
#2284 = AXIS2_PLACEMENT_3D ( 'NONE', #6292, #14222, #2601 ) ;
#2285 = CARTESIAN_POINT ( 'NONE',  ( -4.197393957002300446, -7.680494662014190109E-14, -3.503767560748928922 ) ) ;
#2286 = ORIENTED_EDGE ( 'NONE', *, *, #3854, .F. ) ;
#2287 = CYLINDRICAL_SURFACE ( 'NONE', #10312, 63.00000000000000000 ) ;
#2288 = CARTESIAN_POINT ( 'NONE',  ( 32.92366211674485754, 95.48362627681292736, 15.74283067514923395 ) ) ;
#2289 = ORIENTED_EDGE ( 'NONE', *, *, #8692, .T. ) ;
#2290 = FACE_OUTER_BOUND ( 'NONE', #14783, .T. ) ;
#2291 = DIRECTION ( 'NONE',  ( 1.000000000000000000, 0.000000000000000000, 0.000000000000000000 ) ) ;
#2292 = DIRECTION ( 'NONE',  ( -1.000000000000000000, 0.000000000000000000, 0.000000000000000000 ) ) ;
#2293 = CARTESIAN_POINT ( 'NONE',  ( -53.63365512954686665, 9.714003807514082212, -8.000000000000000000 ) ) ;
#2294 = VECTOR ( 'NONE', #2942, 1000.000000000000000 ) ;
#2295 = CARTESIAN_POINT ( 'NONE',  ( -3.999999999999998224, 2.511478553582034312, -3.469254451724766319 ) ) ;
#2296 = EDGE_CURVE ( 'NONE', #218, #6283, #9841, .T. ) ;
#2297 = DIRECTION ( 'NONE',  ( -0.000000000000000000, -0.000000000000000000, -1.000000000000000000 ) ) ;
#2298 = ORIENTED_EDGE ( 'NONE', *, *, #2956, .T. ) ;
#2299 = ADVANCED_FACE ( 'NONE', ( #8307 ), #184, .T. ) ;
#2300 = CARTESIAN_POINT ( 'NONE',  ( -47.21331623427138879, -33.48561063518577896, -8.000000000000000000 ) ) ;
#2301 = CARTESIAN_POINT ( 'NONE',  ( -2.449293598294700991E-16, 97.00000000000000000, -13.00000000000000178 ) ) ;
#2302 = AXIS2_PLACEMENT_3D ( 'NONE', #12970, #4702, #14035 ) ;
#2303 = EDGE_CURVE ( 'NONE', #1186, #12429, #6434, .T. ) ;
#2304 = CARTESIAN_POINT ( 'NONE',  ( 0.000000000000000000, 0.000000000000000000, -10.50000000000000000 ) ) ;
#2305 = CIRCLE ( 'NONE', #9079, 22.00000000000001421 ) ;
#2306 = CIRCLE ( 'NONE', #7386, 3.000000000000004441 ) ;
#2307 = VECTOR ( 'NONE', #12695, 1000.000000000000000 ) ;
#2308 = DIRECTION ( 'NONE',  ( -1.000000000000000000, -6.215849497113533642E-14, 0.000000000000000000 ) ) ;
#2309 = ORIENTED_EDGE ( 'NONE', *, *, #6700, .T. ) ;
#2310 = ADVANCED_FACE ( 'NONE', ( #1633 ), #11814, .T. ) ;
#2311 = CARTESIAN_POINT ( 'NONE',  ( 0.000000000000000000, 0.000000000000000000, -0.3080913168122742518 ) ) ;
#2312 = ORIENTED_EDGE ( 'NONE', *, *, #2949, .F. ) ;
#2313 = CARTESIAN_POINT ( 'NONE',  ( -12.86891638962156215, 56.43380494353993271, -8.000000000000000000 ) ) ;
#2314 = AXIS2_PLACEMENT_3D ( 'NONE', #10638, #10722, #13078 ) ;
#2315 = DIRECTION ( 'NONE',  ( 0.000000000000000000, 0.000000000000000000, 1.000000000000000000 ) ) ;
#2316 = CARTESIAN_POINT ( 'NONE',  ( 46.81487971942603110, -26.01305530232578533, -10.50000000000000000 ) ) ;
#2317 = ADVANCED_FACE ( 'NONE', ( #4979, #9587 ), #3835, .T. ) ;
#2318 = ORIENTED_EDGE ( 'NONE', *, *, #3202, .F. ) ;
#2319 = EDGE_CURVE ( 'NONE', #8810, #8589, #5422, .T. ) ;
#2320 = CARTESIAN_POINT ( 'NONE',  ( -8.076072847916480058, 62.48290708766281654, -19.99999999999999289 ) ) ;
#2321 = LINE ( 'NONE', #1259, #7864 ) ;
#2322 = CARTESIAN_POINT ( 'NONE',  ( -30.80502811811232888, -49.00442420935981147, 10.49999999999999822 ) ) ;
#2323 = ORIENTED_EDGE ( 'NONE', *, *, #2869, .T. ) ;
#2324 = VECTOR ( 'NONE', #7884, 1000.000000000000000 ) ;
#2325 = VERTEX_POINT ( 'NONE', #8825 ) ;
#2326 = VERTEX_POINT ( 'NONE', #5270 ) ;
#2327 = B_SPLINE_CURVE_WITH_KNOTS ( 'NONE', 3,
 ( #4036, #7359, #1606, #537, #5167, #457, #5089, #11943 ),
 .UNSPECIFIED., .F., .F.,
 ( 4, 2, 2, 4 ),
 ( 2.465131517396147670E-07, 0.001183067374689869729, 0.001774477805458935225, 0.002365888236228000721 ),
 .UNSPECIFIED. ) ;
#2328 = CARTESIAN_POINT ( 'NONE',  ( -65.58935777509570642, -68.58935777509452691, 8.000000000000000000 ) ) ;
#2329 = DIRECTION ( 'NONE',  ( 1.000000000000000000, 0.000000000000000000, 0.000000000000000000 ) ) ;
#2330 = FACE_OUTER_BOUND ( 'NONE', #5410, .T. ) ;
#2331 = CARTESIAN_POINT ( 'NONE',  ( -47.21331623427138879, -33.48561063518577896, -10.50000000000000000 ) ) ;
#2332 = AXIS2_PLACEMENT_3D ( 'NONE', #3686, #7078, #12043 ) ;
#2333 = VERTEX_POINT ( 'NONE', #10962 ) ;
#2334 = DIRECTION ( 'NONE',  ( -1.000000000000000000, 0.000000000000000000, 0.000000000000000000 ) ) ;
#2335 = VERTEX_POINT ( 'NONE', #8674 ) ;
#2336 = CARTESIAN_POINT ( 'NONE',  ( 4.024499207728847949, 2.323545700935682579, -3.572172305156875005 ) ) ;
#2337 = DIRECTION ( 'NONE',  ( -0.000000000000000000, -0.000000000000000000, -1.000000000000000000 ) ) ;
#2338 = ORIENTED_EDGE ( 'NONE', *, *, #9963, .T. ) ;
#2339 = ORIENTED_EDGE ( 'NONE', *, *, #9758, .F. ) ;
#2340 = CARTESIAN_POINT ( 'NONE',  ( 2.500000000000002220, 0.000000000000000000, 0.000000000000000000 ) ) ;
#2341 = AXIS2_PLACEMENT_3D ( 'NONE', #12626, #3296, #12555 ) ;
#2342 = ORIENTED_EDGE ( 'NONE', *, *, #9893, .T. ) ;
#2343 = CARTESIAN_POINT ( 'NONE',  ( -56.43380494354004639, -12.86891638962099549, 8.000000000000000000 ) ) ;
#2344 = CARTESIAN_POINT ( 'NONE',  ( 2.500000000000002220, 2.357898499370430834, -6.938893903907228378E-15 ) ) ;
#2345 = LINE ( 'NONE', #8039, #3777 ) ;
#2346 = CARTESIAN_POINT ( 'NONE',  ( -1.360585162435266282, 4.061296242128070944, -3.505054077164856619 ) ) ;
#2347 = ORIENTED_EDGE ( 'NONE', *, *, #10554, .F. ) ;
#2348 = DIRECTION ( 'NONE',  ( 1.000000000000000000, 0.000000000000000000, 0.000000000000000000 ) ) ;
#2349 = ORIENTED_EDGE ( 'NONE', *, *, #3311, .T. ) ;
#2350 = CARTESIAN_POINT ( 'NONE',  ( 22.33583958711425055, -30.74264578624780597, -28.00000000000000000 ) ) ;
#2351 = EDGE_CURVE ( 'NONE', #3975, #13877, #10329, .T. ) ;
#2352 = ORIENTED_EDGE ( 'NONE', *, *, #665, .F. ) ;
#2353 = CYLINDRICAL_SURFACE ( 'NONE', #5700, 3.000000000000002665 ) ;
#2354 = EDGE_CURVE ( 'NONE', #13011, #7502, #12529, .T. ) ;
#2355 = ADVANCED_FACE ( 'NONE', ( #1917 ), #3074, .T. ) ;
#2356 = ORIENTED_EDGE ( 'NONE', *, *, #9588, .T. ) ;
#2357 = DIRECTION ( 'NONE',  ( 0.000000000000000000, 0.000000000000000000, -1.000000000000000000 ) ) ;
#2358 = ORIENTED_EDGE ( 'NONE', *, *, #5046, .F. ) ;
#2359 = EDGE_CURVE ( 'NONE', #10315, #4701, #10405, .T. ) ;
#2360 = CARTESIAN_POINT ( 'NONE',  ( 50.13108361037843252, 56.43380494353993271, -13.00000000000000178 ) ) ;
#2361 = CARTESIAN_POINT ( 'NONE',  ( -32.39328945491989487, 42.64958156413685941, -10.50000000000000000 ) ) ;
#2362 = CARTESIAN_POINT ( 'NONE',  ( -11.83526203526748333, 106.3435961965382290, 17.51264358390113784 ) ) ;
#2363 = DIRECTION ( 'NONE',  ( -1.000000000000000000, 0.000000000000000000, 0.000000000000000000 ) ) ;
#2364 = DIRECTION ( 'NONE',  ( 1.000000000000000000, 0.000000000000000000, 0.000000000000000000 ) ) ;
#2365 = ITEM_DEFINED_TRANSFORMATION ( 'NONE', 'NONE', #9191,  #5108 ) ;
#2366 = DIRECTION ( 'NONE',  ( 0.000000000000000000, 0.000000000000000000, -1.000000000000000000 ) ) ;
#2367 = ORIENTED_EDGE ( 'NONE', *, *, #6018, .F. ) ;
#2368 = DIRECTION ( 'NONE',  ( 0.000000000000000000, -1.000000000000000000, 0.000000000000000000 ) ) ;
#2369 = CARTESIAN_POINT ( 'NONE',  ( 97.41488903138106537, -0.2790467552935826934, -13.00000000000000178 ) ) ;
#2370 = CONICAL_SURFACE ( 'NONE', #14495, 5.560781378645573980, 1.221730476396046816 ) ;
#2371 = DIRECTION ( 'NONE',  ( -1.000000000000000000, 0.000000000000000000, 0.000000000000000000 ) ) ;
#2372 = DIRECTION ( 'NONE',  ( 0.000000000000000000, 0.000000000000000000, 1.000000000000000000 ) ) ;
#2373 = ORIENTED_EDGE ( 'NONE', *, *, #9362, .T. ) ;
#2374 = CARTESIAN_POINT ( 'NONE',  ( 55.00000000000000711, 2.516649172247811061E-16, -2.055000000000000160 ) ) ;
#2375 = VERTEX_POINT ( 'NONE', #9731 ) ;
#2376 = EDGE_CURVE ( 'NONE', #12171, #13551, #14692, .T. ) ;
#2377 = CARTESIAN_POINT ( 'NONE',  ( -3.492805317593278058, 46.55633131742322917, -10.50000000000000000 ) ) ;
#2378 = CARTESIAN_POINT ( 'NONE',  ( -3.999999999999997335, 0.3987449864459985394, -0.01220643443059497325 ) ) ;
#2379 = CARTESIAN_POINT ( 'NONE',  ( -9.706953719245875689, -57.06275842387046993, -10.50000000000000000 ) ) ;
#2380 = DIRECTION ( 'NONE',  ( 0.000000000000000000, 0.000000000000000000, -1.000000000000000000 ) ) ;
#2381 = VERTEX_POINT ( 'NONE', #12264 ) ;
#2382 = DIRECTION ( 'NONE',  ( 0.000000000000000000, 0.000000000000000000, 1.000000000000000000 ) ) ;
#2383 = AXIS2_PLACEMENT_3D ( 'NONE', #3577, #3347, #4715 ) ;
#2384 = CARTESIAN_POINT ( 'NONE',  ( -36.14014761921588104, 11.74264578624790190, -28.00000000000000000 ) ) ;
#2385 = CARTESIAN_POINT ( 'NONE',  ( -31.47058823529412663, 102.2673069760056563, -10.99999999999999645 ) ) ;
#2386 = ORIENTED_EDGE ( 'NONE', *, *, #1068, .T. ) ;
#2387 = ORIENTED_EDGE ( 'NONE', *, *, #4129, .T. ) ;
#2388 = ADVANCED_FACE ( 'NONE', ( #6305 ), #7689, .F. ) ;
#2389 = ORIENTED_EDGE ( 'NONE', *, *, #927, .T. ) ;
#2390 = ADVANCED_FACE ( 'NONE', ( #13468 ), #5341, .F. ) ;
#2391 = CYLINDRICAL_SURFACE ( 'NONE', #356, 56.99999999999999289 ) ;
#2392 = CARTESIAN_POINT ( 'NONE',  ( -33.47282819776587814, 39.30189486418276346, -8.000000000000000000 ) ) ;
#2393 = CARTESIAN_POINT ( 'NONE',  ( 3.540020015735463321, 2.810662092923963407, -3.602146406945750279 ) ) ;
#2394 = CYLINDRICAL_SURFACE ( 'NONE', #7407, 2.649999999999985700 ) ;
#2395 = CARTESIAN_POINT ( 'NONE',  ( 4.154306624730760511, -2.398490048084971349, -3.721999068284304713 ) ) ;
#2396 = EDGE_LOOP ( 'NONE', ( #670, #11136, #10551, #12131, #4584, #8503, #11152, #3952, #10673, #5544, #622, #10463 ) ) ;
#2397 = ORIENTED_EDGE ( 'NONE', *, *, #2260, .F. ) ;
#2398 = EDGE_CURVE ( 'NONE', #6631, #9297, #8879, .T. ) ;
#2399 = LINE ( 'NONE', #10383, #849 ) ;
#2400 = CIRCLE ( 'NONE', #11864, 2.055000000000000160 ) ;
#2401 = LINE ( 'NONE', #4836, #6001 ) ;
#2402 = EDGE_LOOP ( 'NONE', ( #501, #12886, #10318, #9422, #14673, #9848 ) ) ;
#2403 = ORIENTED_EDGE ( 'NONE', *, *, #7165, .T. ) ;
#2404 = CARTESIAN_POINT ( 'NONE',  ( 0.000000000000000000, 0.000000000000000000, 8.000000000000000000 ) ) ;
#2405 = STYLED_ITEM ( 'NONE', ( #4687 ), #2214 ) ;
#2406 = VERTEX_POINT ( 'NONE', #4293 ) ;
#2407 = EDGE_CURVE ( 'NONE', #6515, #3692, #13012, .T. ) ;
#2408 = CARTESIAN_POINT ( 'NONE',  ( 6.917888187663118416, 52.54657765281190507, -10.50000000000000000 ) ) ;
#2409 = AXIS2_PLACEMENT_3D ( 'NONE', #8803, #5540, #10162 ) ;
#2410 = CARTESIAN_POINT ( 'NONE',  ( 2.500000000000002220, 2.357898499370430834, -6.938893903907228378E-15 ) ) ;
#2411 = DIRECTION ( 'NONE',  ( 0.000000000000000000, 0.000000000000000000, 1.000000000000000000 ) ) ;
#2412 = CARTESIAN_POINT ( 'NONE',  ( 0.000000000000000000, 0.000000000000000000, -10.50000000000000000 ) ) ;
#2413 = ORIENTED_EDGE ( 'NONE', *, *, #9779, .T. ) ;
#2414 = CARTESIAN_POINT ( 'NONE',  ( -8.072319373765147077, 74.56485781596312279, -19.97535925451852989 ) ) ;
#2415 = CARTESIAN_POINT ( 'NONE',  ( 36.14014761921570340, 11.74264578624841171, -25.50000000000000355 ) ) ;
#2416 = ORIENTED_EDGE ( 'NONE', *, *, #1704, .F. ) ;
#2417 = DIRECTION ( 'NONE',  ( 1.000000000000000000, 0.000000000000000000, 0.000000000000000000 ) ) ;
#2418 = AXIS2_PLACEMENT_3D ( 'NONE', #10696, #13057, #7265 ) ;
#2419 = EDGE_LOOP ( 'NONE', ( #12280, #10828, #7764, #1399, #5103, #7846 ) ) ;
#2420 = CIRCLE ( 'NONE', #3394, 59.50000000000000000 ) ;
#2421 = AXIS2_PLACEMENT_3D ( 'NONE', #4056, #2684, #3904 ) ;
#2422 = CIRCLE ( 'NONE', #11159, 5.000000000000000888 ) ;
#2423 = ORIENTED_EDGE ( 'NONE', *, *, #11476, .T. ) ;
#2424 = DIRECTION ( 'NONE',  ( 0.000000000000000000, 0.000000000000000000, 1.000000000000000000 ) ) ;
#2425 = DIRECTION ( 'NONE',  ( -0.000000000000000000, -0.000000000000000000, -1.000000000000000000 ) ) ;
#2426 = CARTESIAN_POINT ( 'NONE',  ( 43.30127018922200932, -24.99999999999987210, 8.000000000000000000 ) ) ;
#2427 = CIRCLE ( 'NONE', #8487, 59.50000000000000000 ) ;
#2428 = LINE ( 'NONE', #6912, #2307 ) ;
#2429 = CARTESIAN_POINT ( 'NONE',  ( 89.61631465359468507, -37.12029293941410657, -8.000000000000000000 ) ) ;
#2430 = CARTESIAN_POINT ( 'NONE',  ( 42.50536573064410106, 32.06294366074510549, -10.50000000000000000 ) ) ;
#2431 = AXIS2_PLACEMENT_3D ( 'NONE', #5590, #7498, #969 ) ;
#2432 = CARTESIAN_POINT ( 'NONE',  ( 9.706953719245472456, 57.06275842387054098, -13.00000000000000178 ) ) ;
#2433 = CIRCLE ( 'NONE', #2383, 100.0000000000000000 ) ;
#2434 =( GEOMETRIC_REPRESENTATION_CONTEXT ( 3 ) GLOBAL_UNCERTAINTY_ASSIGNED_CONTEXT ( ( #8676 ) ) GLOBAL_UNIT_ASSIGNED_CONTEXT ( ( #6419, #14489, #1954 ) ) REPRESENTATION_CONTEXT ( 'NONE', 'WORKASPACE' ) );
#2435 = EDGE_CURVE ( 'NONE', #2645, #3692, #645, .T. ) ;
#2436 = CARTESIAN_POINT ( 'NONE',  ( 22.05882352941176094, 71.68269180561141241, 16.00000000000000000 ) ) ;
#2437 = EDGE_CURVE ( 'NONE', #2144, #7876, #662, .T. ) ;
#2438 = ORIENTED_EDGE ( 'NONE', *, *, #8804, .T. ) ;
#2439 = AXIS2_PLACEMENT_3D ( 'NONE', #851, #13368, #9025 ) ;
#2440 = CARTESIAN_POINT ( 'NONE',  ( -12.23689275498546714, 106.2979809871390131, -16.60898801976832573 ) ) ;
#2441 = DIRECTION ( 'NONE',  ( 1.000000000000000000, 0.000000000000000000, 0.000000000000000000 ) ) ;
#2442 = CIRCLE ( 'NONE', #10928, 63.00000000000000000 ) ;
#2443 = DIRECTION ( 'NONE',  ( -1.000000000000000000, 0.000000000000000000, 0.000000000000000000 ) ) ;
#2444 = TOROIDAL_SURFACE ( 'NONE', #513, 2.700000000000000622, 0.2000000000000000111 ) ;
#2445 = DIRECTION ( 'NONE',  ( 0.000000000000000000, 0.000000000000000000, 1.000000000000000000 ) ) ;
#2446 = CIRCLE ( 'NONE', #9956, 3.000000000000002665 ) ;
#2447 = VERTEX_POINT ( 'NONE', #14617 ) ;
#2448 = FACE_OUTER_BOUND ( 'NONE', #10438, .T. ) ;
#2449 = ORIENTED_EDGE ( 'NONE', *, *, #9032, .T. ) ;
#2450 = B_SPLINE_CURVE_WITH_KNOTS ( 'NONE', 3,
 ( #9072, #2249, #12728, #4675, #6864, #3613 ),
 .UNSPECIFIED., .F., .F.,
 ( 4, 2, 4 ),
 ( 0.003358874760055547120, 0.004541967308452095516, 0.005725059856848643478 ),
 .UNSPECIFIED. ) ;
#2451 = PRODUCT_RELATED_PRODUCT_CATEGORY ( 'part', '', ( #7917 ) ) ;
#2452 = LINE ( 'NONE', #4524, #8241 ) ;
#2453 = DIRECTION ( 'NONE',  ( -0.000000000000000000, -0.000000000000000000, 1.000000000000000000 ) ) ;
#2454 = CIRCLE ( 'NONE', #10942, 56.99999999999999289 ) ;
#2455 = CARTESIAN_POINT ( 'NONE',  ( -37.12029293941441210, -89.61631465359452875, 10.49999999999999822 ) ) ;
#2456 = CARTESIAN_POINT ( 'NONE',  ( 37.12029293941315444, -89.61631465359504034, -10.50000000000000000 ) ) ;
#2457 = ADVANCED_FACE ( 'NONE', ( #12403 ), #7457, .T. ) ;
#2458 = ORIENTED_EDGE ( 'NONE', *, *, #348, .T. ) ;
#2459 = CIRCLE ( 'NONE', #276, 44.89637028918153305 ) ;
#2460 = DIRECTION ( 'NONE',  ( 0.000000000000000000, 0.000000000000000000, 1.000000000000000000 ) ) ;
#2461 = CARTESIAN_POINT ( 'NONE',  ( 12.39897948556635754, 61.76783392443436327, 16.00000000000000000 ) ) ;
#2462 = DIRECTION ( 'NONE',  ( 0.000000000000000000, 0.000000000000000000, -1.000000000000000000 ) ) ;
#2463 = ORIENTED_EDGE ( 'NONE', *, *, #4676, .T. ) ;
#2464 = CIRCLE ( 'NONE', #12900, 7.500000000000001776 ) ;
#2465 = ORIENTED_EDGE ( 'NONE', *, *, #4969, .F. ) ;
#2466 = ORIENTED_EDGE ( 'NONE', *, *, #7180, .T. ) ;
#2467 = AXIS2_PLACEMENT_3D ( 'NONE', #12899, #5352, #12342 ) ;
#2468 = CARTESIAN_POINT ( 'NONE',  ( 12.49999999999999645, 106.2673515243510991, 15.33083626825422741 ) ) ;
#2469 = CARTESIAN_POINT ( 'NONE',  ( 5.200000000000006395, 0.000000000000000000, 2.775557561562891351E-14 ) ) ;
#2470 = DIRECTION ( 'NONE',  ( -0.000000000000000000, -0.000000000000000000, -1.000000000000000000 ) ) ;
#2471 = LINE ( 'NONE', #195, #144 ) ;
#2472 = EDGE_LOOP ( 'NONE', ( #3725, #1496, #13388, #10133, #12962, #13056 ) ) ;
#2473 = DIRECTION ( 'NONE',  ( 0.000000000000000000, -0.5000000000000012212, -0.8660254037844380415 ) ) ;
#2474 = VERTEX_POINT ( 'NONE', #5778 ) ;
#2475 = CIRCLE ( 'NONE', #9735, 2.649999999999992806 ) ;
#2476 = ORIENTED_EDGE ( 'NONE', *, *, #9352, .F. ) ;
#2477 = ADVANCED_FACE ( 'NONE', ( #6842 ), #8066, .F. ) ;
#2478 = DIRECTION ( 'NONE',  ( -0.000000000000000000, -0.000000000000000000, -1.000000000000000000 ) ) ;
#2480 = EDGE_CURVE ( 'NONE', #203, #964, #4296, .T. ) ;
#2479 = CARTESIAN_POINT ( 'NONE',  ( 39.66766701456160860, 30.43807145043623308, 8.000000000000000000 ) ) ;
#2481 = EDGE_CURVE ( 'NONE', #10943, #12827, #1856, .T. ) ;
#2482 = CIRCLE ( 'NONE', #6103, 50.00000000000000000 ) ;
#2483 = LINE ( 'NONE', #6591, #1063 ) ;
#2484 = ORIENTED_EDGE ( 'NONE', *, *, #2501, .T. ) ;
#2485 = ORIENTED_EDGE ( 'NONE', *, *, #9718, .F. ) ;
#2486 = CARTESIAN_POINT ( 'NONE',  ( 33.48561063518626923, -47.21331623427104063, -10.50000000000000000 ) ) ;
#2487 = ORIENTED_EDGE ( 'NONE', *, *, #2319, .F. ) ;
#2488 = AXIS2_PLACEMENT_3D ( 'NONE', #14362, #13009, #8440 ) ;
#2489 = DIRECTION ( 'NONE',  ( 1.000000000000000000, 0.000000000000000000, 0.000000000000000000 ) ) ;
#2490 = EDGE_CURVE ( 'NONE', #14675, #13811, #5498, .T. ) ;
#2491 = CARTESIAN_POINT ( 'NONE',  ( -22.33583958711380646, -30.74264578624812927, -25.50000000000000355 ) ) ;
#2492 = CARTESIAN_POINT ( 'NONE',  ( 44.89637028918153305, 5.498219616798048790E-15, -25.50000000000000355 ) ) ;
#2493 = DIRECTION ( 'NONE',  ( -1.000000000000000000, 0.000000000000000000, 0.000000000000000000 ) ) ;
#2494 = ORIENTED_EDGE ( 'NONE', *, *, #4469, .F. ) ;
#2495 = AXIS2_PLACEMENT_3D ( 'NONE', #10665, #6110, #14629 ) ;
#2496 = CARTESIAN_POINT ( 'NONE',  ( -13.35619814848797837, 51.53979475227131246, 10.49999999999999822 ) ) ;
#2497 = CARTESIAN_POINT ( 'NONE',  ( 5.204748896376250896E-15, 85.00000000000000000, 31.00000000000000000 ) ) ;
#2498 = ORIENTED_EDGE ( 'NONE', *, *, #3771, .F. ) ;
#2499 = CARTESIAN_POINT ( 'NONE',  ( 22.33583958711425055, -30.74264578624780597, -25.50000000000000355 ) ) ;
#2500 = AXIS2_PLACEMENT_3D ( 'NONE', #11397, #14104, #13674 ) ;
#2501 = EDGE_CURVE ( 'NONE', #7516, #132, #13264, .T. ) ;
#2502 = EDGE_LOOP ( 'NONE', ( #6535, #8024, #3119, #8972, #6519 ) ) ;
#2503 = CARTESIAN_POINT ( 'NONE',  ( 3.999999999999996447, 0.000000000000000000, 0.000000000000000000 ) ) ;
#2504 = AXIS2_PLACEMENT_3D ( 'NONE', #8156, #1114, #13863 ) ;
#2505 = CARTESIAN_POINT ( 'NONE',  ( -68.09867107463028901, -68.49330278050098286, -13.00000000000000178 ) ) ;
#2506 = ORIENTED_EDGE ( 'NONE', *, *, #14971, .F. ) ;
#2507 = CARTESIAN_POINT ( 'NONE',  ( 4.211140560182194292, 2.431303136016534250, -3.745885042887433958 ) ) ;
#2508 = CIRCLE ( 'NONE', #1285, 2.700000000000000622 ) ;
#2509 = DIRECTION ( 'NONE',  ( -0.9396926207859138680, 0.000000000000000000, -0.3420201433256536139 ) ) ;
#2510 = VERTEX_POINT ( 'NONE', #13849 ) ;
#2511 = DIRECTION ( 'NONE',  ( -0.000000000000000000, -0.000000000000000000, 1.000000000000000000 ) ) ;
#2512 = DIRECTION ( 'NONE',  ( 0.000000000000000000, 0.000000000000000000, -1.000000000000000000 ) ) ;
#2513 = CARTESIAN_POINT ( 'NONE',  ( -4.197477534772231067, 0.8522413273724359639, -3.505042416683227025 ) ) ;
#2514 = ORIENTED_EDGE ( 'NONE', *, *, #14240, .F. ) ;
#2515 = AXIS2_PLACEMENT_3D ( 'NONE', #4504, #13763, #6908 ) ;
#2516 = CARTESIAN_POINT ( 'NONE',  ( -53.26842454702436669, -11.55014193876159645, 8.000000000000000000 ) ) ;
#2517 = AXIS2_PLACEMENT_3D ( 'NONE', #8968, #11342, #11700 ) ;
#2518 = VERTEX_POINT ( 'NONE', #13695 ) ;
#2519 = CARTESIAN_POINT ( 'NONE',  ( 1.312671235360371558, 3.860931062424218574, -0.05923475698270420919 ) ) ;
#2520 = CARTESIAN_POINT ( 'NONE',  ( 8.915162460657667154, 94.58113943660329426, -19.80393736615727462 ) ) ;
#2521 = DIRECTION ( 'NONE',  ( -0.000000000000000000, 0.000000000000000000, 1.000000000000000000 ) ) ;
#2522 = DIRECTION ( 'NONE',  ( -0.000000000000000000, -0.000000000000000000, 1.000000000000000000 ) ) ;
#2523 = ORIENTED_EDGE ( 'NONE', *, *, #12524, .F. ) ;
#2524 = AXIS2_PLACEMENT_3D ( 'NONE', #11645, #3668, #12703 ) ;
#2525 = ADVANCED_FACE ( 'NONE', ( #12702 ), #11344, .T. ) ;
#2526 = AXIS2_PLACEMENT_3D ( 'NONE', #4425, #5843, #78 ) ;
#2527 = CIRCLE ( 'NONE', #13444, 0.5000000000000004441 ) ;
#2528 = DIRECTION ( 'NONE',  ( -0.000000000000000000, -0.000000000000000000, 1.000000000000000000 ) ) ;
#2529 = CIRCLE ( 'NONE', #594, 46.33974596215558961 ) ;
#2530 = VERTEX_POINT ( 'NONE', #4358 ) ;
#2531 = CARTESIAN_POINT ( 'NONE',  ( 0.000000000000000000, 0.000000000000000000, -8.000000000000000000 ) ) ;
#2532 = DIRECTION ( 'NONE',  ( 0.000000000000000000, 0.000000000000000000, 1.000000000000000000 ) ) ;
#2533 = DIRECTION ( 'NONE',  ( 0.000000000000000000, 0.000000000000000000, 1.000000000000000000 ) ) ;
#2534 = DIRECTION ( 'NONE',  ( 0.000000000000000000, 0.000000000000000000, 1.000000000000000000 ) ) ;
#2535 = CIRCLE ( 'NONE', #5687, 3.000000000000002665 ) ;
#2536 = ORIENTED_EDGE ( 'NONE', *, *, #9431, .T. ) ;
#2537 = ORIENTED_EDGE ( 'NONE', *, *, #3799, .T. ) ;
#2538 = AXIS2_PLACEMENT_3D ( 'NONE', #5505, #11432, #4302 ) ;
#2539 = VECTOR ( 'NONE', #1334, 1000.000000000000000 ) ;
#2540 = LINE ( 'NONE', #1553, #8387 ) ;
#2541 = CARTESIAN_POINT ( 'NONE',  ( -89.33979373934396051, 36.70371619500605220, -13.00000000000000178 ) ) ;
#2542 = CIRCLE ( 'NONE', #8844, 3.000000000000004441 ) ;
#2543 = DIRECTION ( 'NONE',  ( 0.000000000000000000, 0.000000000000000000, 1.000000000000000000 ) ) ;
#2544 = ORIENTED_EDGE ( 'NONE', *, *, #14530, .F. ) ;
#2545 = EDGE_CURVE ( 'NONE', #14464, #13630, #10827, .T. ) ;
#2546 = VERTEX_POINT ( 'NONE', #4579 ) ;
#2547 = EDGE_CURVE ( 'NONE', #9310, #8180, #6208, .T. ) ;
#2548 = EDGE_CURVE ( 'NONE', #13523, #6561, #6695, .T. ) ;
#2549 = CIRCLE ( 'NONE', #12995, 52.50000000000000711 ) ;
#2550 = ORIENTED_EDGE ( 'NONE', *, *, #1572, .F. ) ;
#2551 = AXIS2_PLACEMENT_3D ( 'NONE', #6927, #8075, #1176 ) ;
#2552 = CARTESIAN_POINT ( 'NONE',  ( 10.00610186947451830, 106.5314655734665052, 19.33904518629107017 ) ) ;
#2553 = CONICAL_SURFACE ( 'NONE', #13470, 18.00000000000000355, 0.7853981633974439491 ) ;
#2554 = LINE ( 'NONE', #9232, #7528 ) ;
#2555 = FACE_OUTER_BOUND ( 'NONE', #13595, .T. ) ;
#2556 = SURFACE_STYLE_USAGE ( .BOTH. , #194 ) ;
#2557 = DIRECTION ( 'NONE',  ( 1.000000000000000000, 0.000000000000000000, 0.000000000000000000 ) ) ;
#2558 = EDGE_LOOP ( 'NONE', ( #13037, #3073, #1632, #13708 ) ) ;
#2559 = EDGE_LOOP ( 'NONE', ( #11028, #2465, #5405, #2682, #6596 ) ) ;
#2560 = AXIS2_PLACEMENT_3D ( 'NONE', #13328, #5513, #4380 ) ;
#2561 = DIRECTION ( 'NONE',  ( 0.000000000000000000, 0.000000000000000000, -1.000000000000000000 ) ) ;
#2562 = DIRECTION ( 'NONE',  ( -1.000000000000000000, 0.000000000000000000, 0.000000000000000000 ) ) ;
#2563 = PRESENTATION_LAYER_ASSIGNMENT (  '', '', ( #7888 ) ) ;
#2564 = CARTESIAN_POINT ( 'NONE',  ( 25.00000000000000000, 81.24038404635960831, -23.50000000000000000 ) ) ;
#2565 = VERTEX_POINT ( 'NONE', #11503 ) ;
#2566 = VERTEX_POINT ( 'NONE', #5495 ) ;
#2567 = DIRECTION ( 'NONE',  ( 1.000000000000000000, 0.000000000000000000, 0.000000000000000000 ) ) ;
#2568 = VERTEX_POINT ( 'NONE', #11420 ) ;
#2569 = AXIS2_PLACEMENT_3D ( 'NONE', #11362, #10434, #14857 ) ;
#2570 = CARTESIAN_POINT ( 'NONE',  ( -12.86891638962156215, 56.43380494353993271, -13.00000000000000178 ) ) ;
#2571 = ADVANCED_FACE ( 'NONE', ( #14913, #7835 ), #6920, .F. ) ;
#2572 = CARTESIAN_POINT ( 'NONE',  ( 38.79014761921568777, 11.74264578624841171, -25.50000000000000355 ) ) ;
#2573 = CARTESIAN_POINT ( 'NONE',  ( -25.00000000000000000, 81.24038404635962252, 23.50000000000000355 ) ) ;
#2574 = DIRECTION ( 'NONE',  ( 0.9557692240748189016, 0.2941176470588237613, 0.000000000000000000 ) ) ;
#2575 = DIRECTION ( 'NONE',  ( 0.000000000000000000, 0.000000000000000000, 1.000000000000000000 ) ) ;
#2576 = EDGE_CURVE ( 'NONE', #4454, #1517, #13993, .T. ) ;
#2577 = ORIENTED_EDGE ( 'NONE', *, *, #10702, .F. ) ;
#2578 = DIRECTION ( 'NONE',  ( 0.000000000000000000, 0.000000000000000000, 1.000000000000000000 ) ) ;
#2579 = AXIS2_PLACEMENT_3D ( 'NONE', #1536, #1236, #14219 ) ;
#2580 = ORIENTED_EDGE ( 'NONE', *, *, #11505, .T. ) ;
#2581 = EDGE_LOOP ( 'NONE', ( #13598, #11519, #2403, #12666 ) ) ;
#2582 = CARTESIAN_POINT ( 'NONE',  ( 39.61975340586555916, 91.27544013909752607, 8.000000000000000000 ) ) ;
#2583 = ORIENTED_EDGE ( 'NONE', *, *, #1875, .F. ) ;
#2584 = CARTESIAN_POINT ( 'NONE',  ( 2.500000000000002220, 2.357898499370430834, -6.938893903907228378E-15 ) ) ;
#2585 = CARTESIAN_POINT ( 'NONE',  ( 33.82975856321728969, 101.3925934381291256, -15.34957766734057927 ) ) ;
#2586 = EDGE_CURVE ( 'NONE', #1338, #9298, #8638, .T. ) ;
#2587 = EDGE_CURVE ( 'NONE', #6805, #10315, #7981, .T. ) ;
#2588 = DIRECTION ( 'NONE',  ( 0.000000000000000000, 0.4999999999999997780, -0.8660254037844387076 ) ) ;
#2589 = CYLINDRICAL_SURFACE ( 'NONE', #13842, 3.000000000000002665 ) ;
#2590 = DIRECTION ( 'NONE',  ( -0.000000000000000000, -0.000000000000000000, -1.000000000000000000 ) ) ;
#2591 = VECTOR ( 'NONE', #8974, 1000.000000000000000 ) ;
#2592 = B_SPLINE_CURVE_WITH_KNOTS ( 'NONE', 3,
 ( #5977, #14390, #5128, #2923, #1430, #10541, #3997, #9825, #12192, #10609 ),
 .UNSPECIFIED., .F., .F.,
 ( 4, 2, 2, 2, 4 ),
 ( 0.000000000000000000, 0.001711864931188370777, 0.003423729862376741553, 0.005135594793565112330, 0.006847459724753483107 ),
 .UNSPECIFIED. ) ;
#2593 = DIRECTION ( 'NONE',  ( 1.000000000000000000, 0.000000000000000000, 0.000000000000000000 ) ) ;
#2594 = VERTEX_POINT ( 'NONE', #5714 ) ;
#2595 = DIRECTION ( 'NONE',  ( 0.000000000000000000, 0.000000000000000000, -1.000000000000000000 ) ) ;
#2596 = EDGE_LOOP ( 'NONE', ( #6203, #15002, #8892, #8727, #10518 ) ) ;
#2597 = EDGE_CURVE ( 'NONE', #12895, #1468, #14761, .T. ) ;
#2598 = CARTESIAN_POINT ( 'NONE',  ( -26.24999999999972289, -45.46633369868319363, -10.50000000000000000 ) ) ;
#2599 = DIRECTION ( 'NONE',  ( 1.000000000000000000, 0.000000000000000000, 0.000000000000000000 ) ) ;
#2600 = CARTESIAN_POINT ( 'NONE',  ( -27.94117647058823550, 90.79807628710781842, -23.50000000000000000 ) ) ;
#2601 = DIRECTION ( 'NONE',  ( 0.000000000000000000, 0.000000000000000000, 1.000000000000000000 ) ) ;
#2602 = EDGE_LOOP ( 'NONE', ( #2416, #1965, #8771, #177, #6324 ) ) ;
#2603 = CARTESIAN_POINT ( 'NONE',  ( 30.80502811811196295, 49.00442420936003174, -8.000000000000000000 ) ) ;
#2604 = EDGE_LOOP ( 'NONE', ( #13206, #10127, #419, #9359 ) ) ;
#2605 = EDGE_CURVE ( 'NONE', #14446, #14518, #13610, .T. ) ;
#2606 = EDGE_LOOP ( 'NONE', ( #6975, #3081, #3763, #4083, #1138 ) ) ;
#2607 = DIRECTION ( 'NONE',  ( 0.2941176470588234837, 0.9557692240748187906, 0.000000000000000000 ) ) ;
#2608 = DIRECTION ( 'NONE',  ( 0.000000000000000000, 0.000000000000000000, 1.000000000000000000 ) ) ;
#2609 = CARTESIAN_POINT ( 'NONE',  ( -31.95875033779847030, 102.1112180006092842, -13.22918226575833955 ) ) ;
#2610 = CARTESIAN_POINT ( 'NONE',  ( 0.000000000000000000, 0.000000000000000000, 8.000000000000000000 ) ) ;
#2611 = VECTOR ( 'NONE', #3402, 1000.000000000000000 ) ;
#2612 = ORIENTED_EDGE ( 'NONE', *, *, #12954, .F. ) ;
#2613 = DIRECTION ( 'NONE',  ( -0.000000000000000000, -0.000000000000000000, 1.000000000000000000 ) ) ;
#2614 = FACE_OUTER_BOUND ( 'NONE', #10775, .T. ) ;
#2615 = APPLICATION_CONTEXT ( 'automotive_design' ) ;
#2616 = CARTESIAN_POINT ( 'NONE',  ( 52.36539807335608288, -6.451868917687384020, 10.49999999999999822 ) ) ;
#2617 = EDGE_LOOP ( 'NONE', ( #821, #14798, #4546 ) ) ;
#2618 = VERTEX_POINT ( 'NONE', #12484 ) ;
#2619 = AXIS2_PLACEMENT_3D ( 'NONE', #4922, #4696, #9383 ) ;
#2620 = DIRECTION ( 'NONE',  ( 0.000000000000000000, 0.000000000000000000, 1.000000000000000000 ) ) ;
#2621 = EDGE_LOOP ( 'NONE', ( #13318, #126, #7456, #6714 ) ) ;
#2622 = CYLINDRICAL_SURFACE ( 'NONE', #3768, 100.0000000000000000 ) ;
#2623 = DIRECTION ( 'NONE',  ( -0.8191520442889875797, 1.003171929053519570E-16, 0.5735764363510522656 ) ) ;
#2624 = CARTESIAN_POINT ( 'NONE',  ( -0.02511973781850361173, 4.877415612947412882, -3.751298745799841239 ) ) ;
#2625 = DIRECTION ( 'NONE',  ( 1.000000000000000000, 0.000000000000000000, 0.000000000000000000 ) ) ;
#2626 = EDGE_CURVE ( 'NONE', #13011, #5657, #13755, .T. ) ;
#2627 = EDGE_LOOP ( 'NONE', ( #6115, #8990, #2494, #3096 ) ) ;
#2628 = ORIENTED_EDGE ( 'NONE', *, *, #8795, .T. ) ;
#2629 = EDGE_CURVE ( 'NONE', #11371, #9152, #11813, .T. ) ;
#2630 = ORIENTED_EDGE ( 'NONE', *, *, #7350, .F. ) ;
#2631 = EDGE_CURVE ( 'NONE', #2565, #5824, #3563, .T. ) ;
#2632 = CARTESIAN_POINT ( 'NONE',  ( 68.58935777509475429, -68.58935777509547904, 8.000000000000000000 ) ) ;
#2633 = CARTESIAN_POINT ( 'NONE',  ( -32.26435573746199736, 42.04772703543562073, -10.50000000000000000 ) ) ;
#2634 = DIRECTION ( 'NONE',  ( 1.000000000000000000, 0.000000000000000000, 0.000000000000000000 ) ) ;
#2635 = ORIENTED_EDGE ( 'NONE', *, *, #3584, .F. ) ;
#2636 = EDGE_LOOP ( 'NONE', ( #5047, #14707, #8436, #12121 ) ) ;
#2637 = CARTESIAN_POINT ( 'NONE',  ( 0.000000000000000000, 0.000000000000000000, 16.00000000000000000 ) ) ;
#2638 = ADVANCED_FACE ( 'NONE', ( #13075 ), #7366, .T. ) ;
#2639 = ORIENTED_EDGE ( 'NONE', *, *, #4824, .T. ) ;
#2640 = DIRECTION ( 'NONE',  ( -1.000000000000000000, 0.000000000000000000, 0.000000000000000000 ) ) ;
#2641 = CARTESIAN_POINT ( 'NONE',  ( 1.360585162435297590, -4.061296242128142886, -3.505054077164885484 ) ) ;
#2642 = EDGE_CURVE ( 'NONE', #14343, #303, #14282, .T. ) ;
#2643 = CARTESIAN_POINT ( 'NONE',  ( -0.2790467552932217599, 96.58511096861892042, 10.49999999999999822 ) ) ;
#2644 = CIRCLE ( 'NONE', #11138, 100.0000000000000000 ) ;
#2645 = VERTEX_POINT ( 'NONE', #7213 ) ;
#2646 = DIRECTION ( 'NONE',  ( -1.000000000000000000, 0.000000000000000000, 0.000000000000000000 ) ) ;
#2647 = DIRECTION ( 'NONE',  ( -1.000000000000000000, 0.000000000000000000, 0.000000000000000000 ) ) ;
#2648 = EDGE_LOOP ( 'NONE', ( #8451, #9909, #3886 ) ) ;
#2649 = EDGE_CURVE ( 'NONE', #12492, #2144, #4531, .T. ) ;
#2650 = LINE ( 'NONE', #8637, #12132 ) ;
#2651 = ORIENTED_EDGE ( 'NONE', *, *, #11048, .F. ) ;
#2652 = AXIS2_PLACEMENT_3D ( 'NONE', #14630, #14313, #8769 ) ;
#2653 = ORIENTED_EDGE ( 'NONE', *, *, #8327, .T. ) ;
#2654 = DIRECTION ( 'NONE',  ( 0.000000000000000000, 0.000000000000000000, -1.000000000000000000 ) ) ;
#2655 = CIRCLE ( 'NONE', #5080, 63.00000000000000000 ) ;
#2656 = CARTESIAN_POINT ( 'NONE',  ( 51.45950017607693638, -4.121772567811421872, -8.000000000000000000 ) ) ;
#2657 = CARTESIAN_POINT ( 'NONE',  ( 34.64620656398769682, 101.0151817716822933, -15.74933755401541902 ) ) ;
#2658 = DIRECTION ( 'NONE',  ( -0.000000000000000000, -0.000000000000000000, 1.000000000000000000 ) ) ;
#2659 = LINE ( 'NONE', #12082, #8017 ) ;
#2660 = PLANE ( 'NONE',  #10425 ) ;
#2661 = CIRCLE ( 'NONE', #10908, 53.55662432702593634 ) ;
#2662 = CIRCLE ( 'NONE', #3404, 0.5000000000000004441 ) ;
#2663 = CARTESIAN_POINT ( 'NONE',  ( 57.06275842387049835, -9.706953719245678514, -13.00000000000000178 ) ) ;
#2664 = EDGE_LOOP ( 'NONE', ( #8695, #9215 ) ) ;
#2665 = VECTOR ( 'NONE', #12343, 1000.000000000000000 ) ;
#2666 = AXIS2_PLACEMENT_3D ( 'NONE', #8817, #12255, #636 ) ;
#2667 = DIRECTION ( 'NONE',  ( 1.000000000000000000, 0.000000000000000000, 0.000000000000000000 ) ) ;
#2668 = ORIENTED_EDGE ( 'NONE', *, *, #12523, .F. ) ;
#2669 = AXIS2_PLACEMENT_3D ( 'NONE', #8499, #3815, #6216 ) ;
#2670 = DIRECTION ( 'NONE',  ( 1.000000000000000000, 0.000000000000000000, 0.000000000000000000 ) ) ;
#2671 = DIRECTION ( 'NONE',  ( 0.000000000000000000, 0.000000000000000000, 1.000000000000000000 ) ) ;
#2672 = ADVANCED_FACE ( 'NONE', ( #7289 ), #4737, .F. ) ;
#2673 = EDGE_CURVE ( 'NONE', #4759, #7919, #2103, .T. ) ;
#2674 = CYLINDRICAL_SURFACE ( 'NONE', #13644, 2.649999999999985700 ) ;
#2675 = CIRCLE ( 'NONE', #4388, 18.00000000000000355 ) ;
#2676 = CARTESIAN_POINT ( 'NONE',  ( -46.81487971942585347, 26.01305530232610863, -10.50000000000000000 ) ) ;
#2677 = EDGE_CURVE ( 'NONE', #5269, #10950, #13666, .T. ) ;
#2678 = ORIENTED_EDGE ( 'NONE', *, *, #3984, .T. ) ;
#2679 = CIRCLE ( 'NONE', #1465, 0.5000000000000004441 ) ;
#2680 = CARTESIAN_POINT ( 'NONE',  ( -7.500000000000000888, 106.2673515243510991, 20.00000000000000000 ) ) ;
#2681 = AXIS2_PLACEMENT_3D ( 'NONE', #1527, #6141, #11790 ) ;
#2682 = ORIENTED_EDGE ( 'NONE', *, *, #8692, .F. ) ;
#2683 = AXIS2_PLACEMENT_3D ( 'NONE', #2412, #10161, #14809 ) ;
#2684 = DIRECTION ( 'NONE',  ( 0.000000000000000000, 0.000000000000000000, 1.000000000000000000 ) ) ;
#2685 = DIRECTION ( 'NONE',  ( 1.000000000000000000, 0.000000000000000000, 0.000000000000000000 ) ) ;
#2686 = EDGE_CURVE ( 'NONE', #9298, #4338, #10719, .T. ) ;
#2687 = CARTESIAN_POINT ( 'NONE',  ( -25.00000000000000000, 81.24038404635962252, 31.00000000000000000 ) ) ;
#2688 = CARTESIAN_POINT ( 'NONE',  ( 0.000000000000000000, 1.178949249685208533, -2.042000000000002036 ) ) ;
#2689 = CIRCLE ( 'NONE', #6303, 14.00000000000000000 ) ;
#2690 = ORIENTED_EDGE ( 'NONE', *, *, #13768, .T. ) ;
#2691 = CARTESIAN_POINT ( 'NONE',  ( 9.706953719245472456, 57.06275842387054098, -10.50000000000000000 ) ) ;
#2692 = CIRCLE ( 'NONE', #13364, 3.000000000000002665 ) ;
#2693 = FACE_OUTER_BOUND ( 'NONE', #12286, .T. ) ;
#2694 = EDGE_CURVE ( 'NONE', #5971, #7436, #3726, .T. ) ;
#2695 = CIRCLE ( 'NONE', #1731, 3.000000000000002665 ) ;
#2696 = CARTESIAN_POINT ( 'NONE',  ( 65.64523757230274725, 68.01302780753375998, -13.00000000000000178 ) ) ;
#2697 = ORIENTED_EDGE ( 'NONE', *, *, #14317, .T. ) ;
#2698 = CARTESIAN_POINT ( 'NONE',  ( 22.05882352941176094, 71.68269180561141241, -16.00000000000000000 ) ) ;
#2699 = ORIENTED_EDGE ( 'NONE', *, *, #2900, .T. ) ;
#2700 = AXIS2_PLACEMENT_3D ( 'NONE', #5887, #15016, #14794 ) ;
#2701 = CARTESIAN_POINT ( 'NONE',  ( 7.383907457638312799, 52.72775723226772726, -10.50000000000000000 ) ) ;
#2702 = CIRCLE ( 'NONE', #11194, 60.50000000000000000 ) ;
#2703 = DIRECTION ( 'NONE',  ( 1.000000000000000000, 1.003641614261141513E-13, 0.000000000000000000 ) ) ;
#2704 = CIRCLE ( 'NONE', #14342, 60.50000000000000000 ) ;
#2705 = DIRECTION ( 'NONE',  ( 0.000000000000000000, 0.000000000000000000, 1.000000000000000000 ) ) ;
#2706 = CARTESIAN_POINT ( 'NONE',  ( 0.000000000000000000, 0.000000000000000000, 0.000000000000000000 ) ) ;
#2707 = DIRECTION ( 'NONE',  ( -1.000000000000000000, 0.000000000000000000, -0.000000000000000000 ) ) ;
#2708 = ORIENTED_EDGE ( 'NONE', *, *, #6734, .F. ) ;
#2709 = ORIENTED_EDGE ( 'NONE', *, *, #10051, .F. ) ;
#2710 = CARTESIAN_POINT ( 'NONE',  ( -24.98583958711379793, -30.74264578624812927, -25.50000000000000355 ) ) ;
#2711 = DIRECTION ( 'NONE',  ( 0.000000000000000000, 0.000000000000000000, 1.000000000000000000 ) ) ;
#2712 = AXIS2_PLACEMENT_3D ( 'NONE', #4211, #11418, #1016 ) ;
#2713 = DIRECTION ( 'NONE',  ( 1.000000000000000000, 0.000000000000000000, 0.000000000000000000 ) ) ;
#2714 = VERTEX_POINT ( 'NONE', #2598 ) ;
#2715 = CIRCLE ( 'NONE', #13879, 63.00000000000000000 ) ;
#2716 = ORIENTED_EDGE ( 'NONE', *, *, #12994, .F. ) ;
#2717 = DIRECTION ( 'NONE',  ( -1.000000000000000000, 0.000000000000000000, 0.000000000000000000 ) ) ;
#2718 = ORIENTED_EDGE ( 'NONE', *, *, #14425, .T. ) ;
#2719 = ADVANCED_FACE ( 'NONE', ( #11798 ), #8289, .T. ) ;
#2720 = CARTESIAN_POINT ( 'NONE',  ( -12.39897948556635754, 73.96800191783272282, 16.00000000000000000 ) ) ;
#2721 = EDGE_CURVE ( 'NONE', #10576, #14940, #14512, .T. ) ;
#2722 = CIRCLE ( 'NONE', #14574, 3.000000000000002665 ) ;
#2723 = CARTESIAN_POINT ( 'NONE',  ( 0.000000000000000000, 0.000000000000000000, -8.000000000000000000 ) ) ;
#2724 = ORIENTED_EDGE ( 'NONE', *, *, #14365, .T. ) ;
#2725 = DIRECTION ( 'NONE',  ( 0.000000000000000000, 0.000000000000000000, 1.000000000000000000 ) ) ;
#2726 = DIRECTION ( 'NONE',  ( -1.000000000000000000, 0.000000000000000000, 0.000000000000000000 ) ) ;
#2727 = CIRCLE ( 'NONE', #13165, 2.649999999999985700 ) ;
#2728 = ORIENTED_EDGE ( 'NONE', *, *, #8981, .T. ) ;
#2729 = CYLINDRICAL_SURFACE ( 'NONE', #11396, 0.5000000000000022204 ) ;
#2730 = ORIENTED_EDGE ( 'NONE', *, *, #13517, .F. ) ;
#2731 = VECTOR ( 'NONE', #13721, 1000.000000000000114 ) ;
#2732 = VERTEX_POINT ( 'NONE', #12089 ) ;
#2733 = CARTESIAN_POINT ( 'NONE',  ( 0.000000000000000000, 0.000000000000000000, -10.50000000000000000 ) ) ;
#2734 = AXIS2_PLACEMENT_3D ( 'NONE', #11108, #11495, #2363 ) ;
#2735 = ADVANCED_FACE ( 'NONE', ( #7507 ), #8881, .T. ) ;
#2736 = EDGE_CURVE ( 'NONE', #11234, #6805, #4051, .T. ) ;
#2737 = DIRECTION ( 'NONE',  ( 0.000000000000000000, 0.000000000000000000, 1.000000000000000000 ) ) ;
#2738 = CARTESIAN_POINT ( 'NONE',  ( 36.52608637591580987, -92.55687898036917716, 8.000000000000000000 ) ) ;
#2739 = CARTESIAN_POINT ( 'NONE',  ( -89.61631465359519666, -37.12029293941281338, -13.00000000000000178 ) ) ;
#2740 = DIRECTION ( 'NONE',  ( 0.000000000000000000, 0.000000000000000000, 1.000000000000000000 ) ) ;
#2741 = DIRECTION ( 'NONE',  ( 0.000000000000000000, 0.000000000000000000, 1.000000000000000000 ) ) ;
#2742 = AXIS2_PLACEMENT_3D ( 'NONE', #7838, #11050, #5199 ) ;
#2743 = VERTEX_POINT ( 'NONE', #12164 ) ;
#2744 = CARTESIAN_POINT ( 'NONE',  ( 50.00000000000000000, -6.123233995736766085E-15, -13.00000000000000178 ) ) ;
#2745 = ORIENTED_EDGE ( 'NONE', *, *, #12331, .F. ) ;
#2746 = DIRECTION ( 'NONE',  ( -0.000000000000000000, -0.000000000000000000, 1.000000000000000000 ) ) ;
#2747 = DIRECTION ( 'NONE',  ( 0.000000000000000000, 0.000000000000000000, 1.000000000000000000 ) ) ;
#2748 = CIRCLE ( 'NONE', #10742, 0.5000000000000004441 ) ;
#2749 = DIRECTION ( 'NONE',  ( -0.000000000000000000, -0.000000000000000000, -1.000000000000000000 ) ) ;
#2750 = CARTESIAN_POINT ( 'NONE',  ( 97.00000000000000000, -3.384287605079545030E-13, -13.00000000000000178 ) ) ;
#2751 = AXIS2_PLACEMENT_3D ( 'NONE', #13758, #2129, #14743 ) ;
#2752 = VERTEX_POINT ( 'NONE', #3966 ) ;
#2753 = DIRECTION ( 'NONE',  ( 1.000000000000000000, 0.000000000000000000, 0.000000000000000000 ) ) ;
#2754 = ORIENTED_EDGE ( 'NONE', *, *, #9125, .F. ) ;
#2755 = ORIENTED_EDGE ( 'NONE', *, *, #2303, .T. ) ;
#2756 = CARTESIAN_POINT ( 'NONE',  ( 30.00000000000001066, 97.48846085563154418, -26.00000000000000000 ) ) ;
#2757 = DIRECTION ( 'NONE',  ( 1.000000000000000000, 0.000000000000000000, 0.000000000000000000 ) ) ;
#2758 = AXIS2_PLACEMENT_3D ( 'NONE', #1865, #4149, #3156 ) ;
#2759 = CARTESIAN_POINT ( 'NONE',  ( -31.47058823529412663, 102.2673069760056563, -10.99999999999999645 ) ) ;
#2760 = EDGE_CURVE ( 'NONE', #5754, #9386, #14476, .T. ) ;
#2761 = DIRECTION ( 'NONE',  ( 1.000000000000000000, 0.000000000000000000, 0.000000000000000000 ) ) ;
#2762 = DIRECTION ( 'NONE',  ( 0.000000000000000000, 0.000000000000000000, 1.000000000000000000 ) ) ;
#2763 = EDGE_CURVE ( 'NONE', #4112, #1683, #14226, .T. ) ;
#2764 = VERTEX_POINT ( 'NONE', #2970 ) ;
#2765 = CARTESIAN_POINT ( 'NONE',  ( -42.04772703543551415, -32.26435573746212526, 10.49999999999999822 ) ) ;
#2766 = LINE ( 'NONE', #5196, #7374 ) ;
#2767 = AXIS2_PLACEMENT_3D ( 'NONE', #13469, #7613, #12556 ) ;
#2768 = DIRECTION ( 'NONE',  ( 0.000000000000000000, 0.000000000000000000, 1.000000000000000000 ) ) ;
#2769 = VECTOR ( 'NONE', #778, 1000.000000000000000 ) ;
#2770 = CIRCLE ( 'NONE', #11262, 20.00000000000000000 ) ;
#2771 = EDGE_CURVE ( 'NONE', #5876, #3028, #11579, .T. ) ;
#2772 = VERTEX_POINT ( 'NONE', #5252 ) ;
#2773 = DIRECTION ( 'NONE',  ( -1.000000000000000000, 0.000000000000000000, 0.000000000000000000 ) ) ;
#2774 = ORIENTED_EDGE ( 'NONE', *, *, #1522, .T. ) ;
#2775 = DIRECTION ( 'NONE',  ( 0.000000000000000000, 0.000000000000000000, 1.000000000000000000 ) ) ;
#2776 = ORIENTED_EDGE ( 'NONE', *, *, #1912, .F. ) ;
#2777 = ADVANCED_FACE ( 'NONE', ( #7591 ), #1680, .F. ) ;
#2778 = AXIS2_PLACEMENT_3D ( 'NONE', #9675, #8979, #13540 ) ;
#2779 = CARTESIAN_POINT ( 'NONE',  ( 30.80502811811196295, 49.00442420936003174, 10.49999999999999822 ) ) ;
#2780 = EDGE_CURVE ( 'NONE', #13864, #14119, #6287, .T. ) ;
#2781 = CARTESIAN_POINT ( 'NONE',  ( 0.6666666666666654084, -4.233901974057272533, -3.300726591567086921 ) ) ;
#2782 = CARTESIAN_POINT ( 'NONE',  ( -6.938893903907228378E-15, 38.00000000000000000, 19.49999999999999645 ) ) ;
#2783 = DIRECTION ( 'NONE',  ( 0.000000000000000000, 0.000000000000000000, 1.000000000000000000 ) ) ;
#2784 = AXIS2_PLACEMENT_3D ( 'NONE', #11335, #11404, #9186 ) ;
#2785 = AXIS2_PLACEMENT_3D ( 'NONE', #1842, #1770, #6457 ) ;
#2786 = ORIENTED_EDGE ( 'NONE', *, *, #3759, .T. ) ;
#2787 = ORIENTED_EDGE ( 'NONE', *, *, #3434, .T. ) ;
#2788 = CARTESIAN_POINT ( 'NONE',  ( 2.649999999999993250, 38.00000000000000000, -25.50000000000000355 ) ) ;
#2789 = FACE_OUTER_BOUND ( 'NONE', #2606, .T. ) ;
#2790 = B_SPLINE_CURVE_WITH_KNOTS ( 'NONE', 3,
 ( #7719, #8932, #1814, #12362, #7571, #14731, #11001, #9850 ),
 .UNSPECIFIED., .F., .F.,
 ( 4, 2, 2, 4 ),
 ( 2.465131517120941901E-07, 0.001183067374689838070, 0.001774477805458900747, 0.002365888236227963858 ),
 .UNSPECIFIED. ) ;
#2791 = DIRECTION ( 'NONE',  ( 0.000000000000000000, 0.000000000000000000, -1.000000000000000000 ) ) ;
#2792 = ORIENTED_EDGE ( 'NONE', *, *, #5931, .T. ) ;
#2793 = EDGE_CURVE ( 'NONE', #7980, #2928, #8411, .T. ) ;
#2794 = CIRCLE ( 'NONE', #6895, 59.50000000000000000 ) ;
#2795 = ORIENTED_EDGE ( 'NONE', *, *, #937, .F. ) ;
#2796 = FACE_OUTER_BOUND ( 'NONE', #3840, .T. ) ;
#2797 = VECTOR ( 'NONE', #1640, 1000.000000000000000 ) ;
#2798 = AXIS2_PLACEMENT_3D ( 'NONE', #8975, #14838, #2146 ) ;
#2799 = AXIS2_PLACEMENT_3D ( 'NONE', #4648, #11576, #2291 ) ;
#2800 = ORIENTED_EDGE ( 'NONE', *, *, #8886, .F. ) ;
#2801 = DIRECTION ( 'NONE',  ( 0.000000000000000000, 0.000000000000000000, -1.000000000000000000 ) ) ;
#2802 = EDGE_LOOP ( 'NONE', ( #5915, #4773, #8392, #11552 ) ) ;
#2803 = CIRCLE ( 'NONE', #5934, 0.5155456020628804703 ) ;
#2804 = DIRECTION ( 'NONE',  ( -0.000000000000000000, -0.000000000000000000, 1.000000000000000000 ) ) ;
#2805 = DIRECTION ( 'NONE',  ( 1.000000000000000000, 0.000000000000000000, 0.000000000000000000 ) ) ;
#2806 = ORIENTED_EDGE ( 'NONE', *, *, #11216, .T. ) ;
#2807 = DIRECTION ( 'NONE',  ( 1.000000000000000000, 0.000000000000000000, -0.000000000000000000 ) ) ;
#2808 = ORIENTED_EDGE ( 'NONE', *, *, #1188, .F. ) ;
#2809 = EDGE_LOOP ( 'NONE', ( #10413, #11835, #10660, #13459 ) ) ;
#2810 = CARTESIAN_POINT ( 'NONE',  ( -31.32379180359345838, 96.02017129613334134, 14.76790389961145600 ) ) ;
#2811 = VECTOR ( 'NONE', #1270, 1000.000000000000000 ) ;
#2812 = CIRCLE ( 'NONE', #14699, 63.00000000000000000 ) ;
#2813 = DIRECTION ( 'NONE',  ( 1.000000000000000000, 0.000000000000000000, 0.000000000000000000 ) ) ;
#2814 = DIRECTION ( 'NONE',  ( 0.000000000000000000, 0.000000000000000000, -1.000000000000000000 ) ) ;
#2815 = CARTESIAN_POINT ( 'NONE',  ( 89.61631465359468507, -37.12029293941410657, -8.000000000000000000 ) ) ;
#2816 = DIRECTION ( 'NONE',  ( 1.000000000000000000, 0.000000000000000000, 0.000000000000000000 ) ) ;
#2817 = LINE ( 'NONE', #4875, #6994 ) ;
#2818 = ORIENTED_EDGE ( 'NONE', *, *, #13128, .T. ) ;
#2819 = AXIS2_PLACEMENT_3D ( 'NONE', #11738, #4900, #10877 ) ;
#2820 = EDGE_CURVE ( 'NONE', #5837, #8250, #8579, .T. ) ;
#2821 = DIRECTION ( 'NONE',  ( 0.000000000000000000, 0.000000000000000000, 1.000000000000000000 ) ) ;
#2822 = ORIENTED_EDGE ( 'NONE', *, *, #11520, .F. ) ;
#2823 = EDGE_CURVE ( 'NONE', #12895, #14306, #5740, .T. ) ;
#2824 = EDGE_CURVE ( 'NONE', #3692, #13772, #6454, .T. ) ;
#2825 = EDGE_CURVE ( 'NONE', #5327, #198, #1867, .T. ) ;
#2826 = DIRECTION ( 'NONE',  ( 1.000000000000000000, 0.000000000000000000, 0.000000000000000000 ) ) ;
#2827 = DIRECTION ( 'NONE',  ( 0.000000000000000000, 0.000000000000000000, 1.000000000000000000 ) ) ;
#2828 = EDGE_LOOP ( 'NONE', ( #12358, #11033, #10938, #1048 ) ) ;
#2829 = CARTESIAN_POINT ( 'NONE',  ( 29.70588235294119173, 96.53269163155674448, -10.99999999999999645 ) ) ;
#2830 = EDGE_CURVE ( 'NONE', #303, #2935, #3816, .T. ) ;
#2831 = FACE_OUTER_BOUND ( 'NONE', #11343, .T. ) ;
#2832 = ORIENTED_EDGE ( 'NONE', *, *, #4781, .T. ) ;
#2833 = AXIS2_PLACEMENT_3D ( 'NONE', #8438, #11719, #1393 ) ;
#2834 = DIRECTION ( 'NONE',  ( -1.000000000000000000, 0.000000000000000000, 0.000000000000000000 ) ) ;
#2835 = EDGE_LOOP ( 'NONE', ( #1841, #7715, #9592, #11283 ) ) ;
#2836 = CARTESIAN_POINT ( 'NONE',  ( 0.000000000000000000, 0.000000000000000000, 13.00000000000000178 ) ) ;
#2837 = DIRECTION ( 'NONE',  ( -1.000000000000000000, 0.000000000000000000, 0.000000000000000000 ) ) ;
#2838 = CARTESIAN_POINT ( 'NONE',  ( 36.14014761921570340, 11.74264578624841171, -25.50000000000000355 ) ) ;
#2839 = CARTESIAN_POINT ( 'NONE',  ( 55.00000000000000711, 0.000000000000000000, 2.055000000000000160 ) ) ;
#2840 = DIRECTION ( 'NONE',  ( -0.000000000000000000, -0.000000000000000000, 1.000000000000000000 ) ) ;
#2841 = ORIENTED_EDGE ( 'NONE', *, *, #13537, .F. ) ;
#2842 = CARTESIAN_POINT ( 'NONE',  ( 0.000000000000000000, 0.000000000000000000, -5.000000000000000888 ) ) ;
#2843 = DIRECTION ( 'NONE',  ( 1.000000000000000000, 0.000000000000000000, 0.000000000000000000 ) ) ;
#2844 = CARTESIAN_POINT ( 'NONE',  ( 32.26435573746228158, -42.04772703543541468, -8.000000000000000000 ) ) ;
#2845 = EDGE_CURVE ( 'NONE', #11326, #2743, #13668, .T. ) ;
#2846 = ORIENTED_EDGE ( 'NONE', *, *, #7882, .F. ) ;
#2847 = CARTESIAN_POINT ( 'NONE',  ( 0.000000000000000000, 0.000000000000000000, -4.694516984716113228 ) ) ;
#2848 = ORIENTED_EDGE ( 'NONE', *, *, #12480, .F. ) ;
#2849 = DIRECTION ( 'NONE',  ( 1.000000000000000000, 0.000000000000000000, 0.000000000000000000 ) ) ;
#2850 = PLANE ( 'NONE',  #11939 ) ;
#2851 = CARTESIAN_POINT ( 'NONE',  ( 51.53979475227119167, 13.35619814848851483, 10.49999999999999822 ) ) ;
#2852 = CARTESIAN_POINT ( 'NONE',  ( 0.6810597143197147929, 4.461075778259437463, -3.598441714920656676 ) ) ;
#2853 = APPLICATION_PROTOCOL_DEFINITION ( 'draft international standard', 'automotive_design', 1998, #13871 ) ;
#2854 = CARTESIAN_POINT ( 'NONE',  ( -29.73684566822694464, 96.52317875358642141, -11.65491793965443001 ) ) ;
#2855 = VERTEX_POINT ( 'NONE', #4109 ) ;
#2856 = ORIENTED_EDGE ( 'NONE', *, *, #12772, .T. ) ;
#2857 = CARTESIAN_POINT ( 'NONE',  ( -13.21740939043329099, 51.19406879332069593, -10.50000000000000000 ) ) ;
#2858 = DIRECTION ( 'NONE',  ( 1.000000000000000000, 0.000000000000000000, -0.000000000000000000 ) ) ;
#2859 = DIRECTION ( 'NONE',  ( 0.000000000000000000, 0.000000000000000000, -1.000000000000000000 ) ) ;
#2860 = ORIENTED_EDGE ( 'NONE', *, *, #2824, .F. ) ;
#2861 = EDGE_CURVE ( 'NONE', #14730, #11825, #5168, .T. ) ;
#2862 = ADVANCED_FACE ( 'NONE', ( #8807 ), #5401, .T. ) ;
#2863 = ORIENTED_EDGE ( 'NONE', *, *, #8614, .F. ) ;
#2864 = FACE_OUTER_BOUND ( 'NONE', #10048, .T. ) ;
#2865 = ORIENTED_EDGE ( 'NONE', *, *, #8873, .T. ) ;
#2866 = CARTESIAN_POINT ( 'NONE',  ( -48.19406879332065330, -13.71740939043347041, 8.000000000000000000 ) ) ;
#2867 = CARTESIAN_POINT ( 'NONE',  ( 1.257172072275600794, -3.892973519171010643, -3.433252694550598783 ) ) ;
#2868 =( BOUNDED_SURFACE ( )  B_SPLINE_SURFACE ( 3, 2, ( 
 ( #5884, #9301, #13959 ),
 ( #3552, #1053, #2393 ),
 ( #7011, #1268, #123 ),
 ( #9376, #13107, #4914 ),
 ( #1415, #11750, #2852 ),
 ( #6184, #5054, #2624 ) ),
 .UNSPECIFIED., .F., .F., .F. ) 
 B_SPLINE_SURFACE_WITH_KNOTS ( ( 4, 2, 4 ),
 ( 3, 3 ),
 ( 0.02032853247518126225, 0.02278863295364821212, 0.02524873343211516200 ),
 ( 0.000000000000000000, 1.000000000000000000 ),
 .UNSPECIFIED. ) 
 GEOMETRIC_REPRESENTATION_ITEM ( )  RATIONAL_B_SPLINE_SURFACE ( (
 ( 1.000000000000000000, 0.8047781615896835161, 1.000000000000000000),
 ( 1.000000000000000000, 0.8123767586289261100, 1.000000000000000000),
 ( 1.000000000000000000, 0.8190662415564383680, 1.000000000000000000),
 ( 1.000000000000000000, 0.8192361015669021862, 1.000000000000000000),
 ( 1.000000000000000000, 0.8126135807103909148, 1.000000000000000000),
 ( 1.000000000000000000, 0.8047712338318580017, 1.000000000000000000) ) ) 
 REPRESENTATION_ITEM ( '' )  SURFACE ( )  );
#2869 = EDGE_CURVE ( 'NONE', #14637, #14691, #8945, .T. ) ;
#2870 = CARTESIAN_POINT ( 'NONE',  ( -97.41488903138106537, 0.2790467552942557661, 10.49999999999999822 ) ) ;
#2871 = DIRECTION ( 'NONE',  ( 0.000000000000000000, -0.000000000000000000, -1.000000000000000000 ) ) ;
#2872 = EDGE_LOOP ( 'NONE', ( #10619, #5353, #8191, #11115, #887 ) ) ;
#2873 = CYLINDRICAL_SURFACE ( 'NONE', #10654, 3.000000000000002665 ) ;
#2874 = ORIENTED_EDGE ( 'NONE', *, *, #2780, .T. ) ;
#2875 = ADVANCED_FACE ( 'NONE', ( #4422 ), #7346, .T. ) ;
#2876 = VERTEX_POINT ( 'NONE', #11759 ) ;
#2877 = DIRECTION ( 'NONE',  ( -1.000000000000000000, 0.000000000000000000, 0.000000000000000000 ) ) ;
#2878 = VERTEX_POINT ( 'NONE', #7896 ) ;
#2879 = CARTESIAN_POINT ( 'NONE',  ( 35.00000000000000000, 81.24038404635960831, -13.50000000000000178 ) ) ;
#2880 = CARTESIAN_POINT ( 'NONE',  ( -45.88839665196098849, 26.99988008862674960, 10.49999999999999822 ) ) ;
#2881 = CARTESIAN_POINT ( 'NONE',  ( 100.0000000000000000, -3.675178358715236078E-13, -8.000000000000000000 ) ) ;
#2882 = CARTESIAN_POINT ( 'NONE',  ( 35.00000000000000000, 81.24038404635960831, -16.00000000000000000 ) ) ;
#2883 = DIRECTION ( 'NONE',  ( 1.000000000000000000, 0.000000000000000000, 0.000000000000000000 ) ) ;
#2884 = ORIENTED_EDGE ( 'NONE', *, *, #14608, .T. ) ;
#2885 = DIRECTION ( 'NONE',  ( -1.000000000000000000, 0.000000000000000000, 0.000000000000000000 ) ) ;
#2886 = CARTESIAN_POINT ( 'NONE',  ( 9.917888187663120192, 52.54657765281190507, -13.00000000000000178 ) ) ;
#2887 = DIRECTION ( 'NONE',  ( 0.000000000000000000, 0.000000000000000000, -1.000000000000000000 ) ) ;
#2888 = CIRCLE ( 'NONE', #11630, 2.649999999999985700 ) ;
#2889 = FACE_OUTER_BOUND ( 'NONE', #8793, .T. ) ;
#2890 = ORIENTED_EDGE ( 'NONE', *, *, #10068, .T. ) ;
#2891 = CARTESIAN_POINT ( 'NONE',  ( 30.19044911324211711, 96.38232397946876517, -13.21859331841448792 ) ) ;
#2892 = DIRECTION ( 'NONE',  ( 0.000000000000000000, 0.000000000000000000, -1.000000000000000000 ) ) ;
#2893 = ORIENTED_EDGE ( 'NONE', *, *, #7180, .F. ) ;
#2894 = CARTESIAN_POINT ( 'NONE',  ( -12.50000000000000000, 40.62019202317981126, -23.50000000000000000 ) ) ;
#2895 = COLOUR_RGB ( '', 0.72549020, 0.75294118, 0.79215686) ;
#2896 = ORIENTED_EDGE ( 'NONE', *, *, #3604, .T. ) ;
#2897 = AXIS2_PLACEMENT_3D ( 'NONE', #8890, #11104, #936 ) ;
#2898 = DIRECTION ( 'NONE',  ( -0.000000000000000000, -0.000000000000000000, 1.000000000000000000 ) ) ;
#2899 = CARTESIAN_POINT ( 'NONE',  ( 0.000000000000000000, 0.000000000000000000, -8.000000000000000000 ) ) ;
#2900 = EDGE_CURVE ( 'NONE', #5135, #12050, #13419, .T. ) ;
#2901 = DIRECTION ( 'NONE',  ( 0.000000000000000000, 0.000000000000000000, 1.000000000000000000 ) ) ;
#2902 = CIRCLE ( 'NONE', #4367, 100.0000000000000000 ) ;
#2903 = EDGE_CURVE ( 'NONE', #14727, #2447, #12694, .T. ) ;
#2904 = CARTESIAN_POINT ( 'NONE',  ( 37.12029293941315444, -89.61631465359504034, -8.000000000000000000 ) ) ;
#2906 = CARTESIAN_POINT ( 'NONE',  ( 69.08004447556065486, 68.68541276968852571, -10.50000000000000000 ) ) ;
#2905 = CIRCLE ( 'NONE', #2669, 0.5000000000000073275 ) ;
#2907 = DIRECTION ( 'NONE',  ( -0.000000000000000000, -0.000000000000000000, -1.000000000000000000 ) ) ;
#2908 = VERTEX_POINT ( 'NONE', #10253 ) ;
#2909 = ORIENTED_EDGE ( 'NONE', *, *, #13742, .F. ) ;
#2910 = CARTESIAN_POINT ( 'NONE',  ( 0.000000000000000000, 0.000000000000000000, 13.00000000000000178 ) ) ;
#2911 = DIRECTION ( 'NONE',  ( -0.7071067811865444641, 8.659560562354895880E-17, 0.7071067811865505703 ) ) ;
#2912 = VECTOR ( 'NONE', #8588, 1000.000000000000000 ) ;
#2913 = CARTESIAN_POINT ( 'NONE',  ( 56.43380494353997534, 12.86891638962136319, -13.00000000000000178 ) ) ;
#2914 = CIRCLE ( 'NONE', #11410, 53.55662432702593634 ) ;
#2915 = AXIS2_PLACEMENT_3D ( 'NONE', #3829, #7223, #6229 ) ;
#2916 = AXIS2_PLACEMENT_3D ( 'NONE', #2573, #373, #14262 ) ;
#2917 = ORIENTED_EDGE ( 'NONE', *, *, #9425, .F. ) ;
#2918 = EDGE_CURVE ( 'NONE', #14637, #7984, #82, .T. ) ;
#2919 = DIRECTION ( 'NONE',  ( -1.000000000000000000, 0.000000000000000000, 0.000000000000000000 ) ) ;
#2920 = VERTEX_POINT ( 'NONE', #1080 ) ;
#2921 = DIRECTION ( 'NONE',  ( 0.000000000000000000, 0.000000000000000000, -1.000000000000000000 ) ) ;
#2922 = EDGE_CURVE ( 'NONE', #5730, #14727, #7736, .T. ) ;
#2923 = CARTESIAN_POINT ( 'NONE',  ( -9.718176292668218252, 74.36971601906103047, 19.51774219187060311 ) ) ;
#2924 = VECTOR ( 'NONE', #10337, 1000.000000000000227 ) ;
#2925 = LINE ( 'NONE', #5130, #3433 ) ;
#2926 = CARTESIAN_POINT ( 'NONE',  ( -2.449293598294708880E-16, 38.00000000000000000, -25.50000000000000355 ) ) ;
#2927 = PRODUCT_CONTEXT ( 'NONE', #3784, 'mechanical' ) ;
#2928 = VERTEX_POINT ( 'NONE', #11329 ) ;
#2929 = CIRCLE ( 'NONE', #2681, 68.00000000000000000 ) ;
#2930 = ORIENTED_EDGE ( 'NONE', *, *, #8566, .T. ) ;
#2931 = AXIS2_PLACEMENT_3D ( 'NONE', #13516, #12383, #11249 ) ;
#2932 = CARTESIAN_POINT ( 'NONE',  ( -20.00000000000000000, 0.000000000000000000, -25.50000000000000355 ) ) ;
#2933 = CARTESIAN_POINT ( 'NONE',  ( 2.449293598294700991E-16, -97.00000000000000000, 8.000000000000000000 ) ) ;
#2934 = DIRECTION ( 'NONE',  ( -0.000000000000000000, -0.000000000000000000, 1.000000000000000000 ) ) ;
#2935 = VERTEX_POINT ( 'NONE', #9456 ) ;
#2936 = VECTOR ( 'NONE', #11554, 1000.000000000000000 ) ;
#2937 = VERTEX_POINT ( 'NONE', #4498 ) ;
#2938 = ADVANCED_BREP_SHAPE_REPRESENTATION ( '', ( #8964, #5108 ), #14072 ) ;
#2939 = AXIS2_PLACEMENT_3D ( 'NONE', #10520, #13958, #9300 ) ;
#2940 = VERTEX_POINT ( 'NONE', #999 ) ;
#2941 = AXIS2_PLACEMENT_3D ( 'NONE', #11472, #1070, #3264 ) ;
#2942 = DIRECTION ( 'NONE',  ( 0.000000000000000000, 0.000000000000000000, 1.000000000000000000 ) ) ;
#2943 = PLANE ( 'NONE',  #9783 ) ;
#2944 = ADVANCED_FACE ( 'NONE', ( #928 ), #8249, .T. ) ;
#2945 = EDGE_CURVE ( 'NONE', #9923, #1683, #4772, .T. ) ;
#2947 = CIRCLE ( 'NONE', #7291, 63.00000000000000000 ) ;
#2946 = DIRECTION ( 'NONE',  ( -0.000000000000000000, -0.000000000000000000, -1.000000000000000000 ) ) ;
#2948 = CARTESIAN_POINT ( 'NONE',  ( -33.08545438203827871, 101.7020459634811118, 14.77901645503695427 ) ) ;
#2949 = EDGE_CURVE ( 'NONE', #9901, #8073, #2483, .T. ) ;
#2950 = ORIENTED_EDGE ( 'NONE', *, *, #13235, .T. ) ;
#2951 = DIRECTION ( 'NONE',  ( 0.000000000000000000, 0.000000000000000000, 1.000000000000000000 ) ) ;
#2952 = AXIS2_PLACEMENT_3D ( 'NONE', #7806, #6732, #13749 ) ;
#2953 = ORIENTED_EDGE ( 'NONE', *, *, #5003, .T. ) ;
#2954 = ORIENTED_EDGE ( 'NONE', *, *, #3044, .T. ) ;
#2955 = CARTESIAN_POINT ( 'NONE',  ( 57.06275842387049835, -9.706953719245678514, -8.000000000000000000 ) ) ;
#2956 = EDGE_CURVE ( 'NONE', #12263, #218, #13657, .T. ) ;
#2957 = CIRCLE ( 'NONE', #7553, 2.649999999999992806 ) ;
#2958 = FACE_OUTER_BOUND ( 'NONE', #776, .T. ) ;
#2959 = CIRCLE ( 'NONE', #1504, 0.5000000000000022204 ) ;
#2960 = CARTESIAN_POINT ( 'NONE',  ( 0.000000000000000000, 0.000000000000000000, -8.000000000000000000 ) ) ;
#2961 = CARTESIAN_POINT ( 'NONE',  ( -31.74999999999995737, 5.204748896376250699E-16, -4.250000000000028422 ) ) ;
#2962 = LINE ( 'NONE', #5471, #238 ) ;
#2963 = EDGE_CURVE ( 'NONE', #4159, #14486, #8561, .T. ) ;
#2964 = CARTESIAN_POINT ( 'NONE',  ( 49.11971303961677648, 15.88467684210564990, -13.00000000000000178 ) ) ;
#2965 = EDGE_CURVE ( 'NONE', #5889, #13141, #5478, .T. ) ;
#2966 = EDGE_LOOP ( 'NONE', ( #5799, #12449, #1206, #70, #13723, #11353, #13169, #12816, #12321 ) ) ;
#2967 = PLANE ( 'NONE',  #13594 ) ;
#2968 = CARTESIAN_POINT ( 'NONE',  ( 11.55014193876178652, -53.26842454702432406, -13.00000000000000178 ) ) ;
#2969 = AXIS2_PLACEMENT_3D ( 'NONE', #11740, #15008, #3381 ) ;
#2970 = CARTESIAN_POINT ( 'NONE',  ( 24.98583958711423492, -30.74264578624780597, -25.50000000000000355 ) ) ;
#2971 = CARTESIAN_POINT ( 'NONE',  ( 4.197393957002300446, 0.8151795401431369825, -3.503767560748934251 ) ) ;
#2972 = EDGE_LOOP ( 'NONE', ( #3556, #13703, #4163, #793 ) ) ;
#2973 = AXIS2_PLACEMENT_3D ( 'NONE', #10729, #4894, #7152 ) ;
#2974 = ORIENTED_EDGE ( 'NONE', *, *, #5280, .F. ) ;
#2975 = FILL_AREA_STYLE_COLOUR ( '', #12262 ) ;
#2976 = VERTEX_POINT ( 'NONE', #12607 ) ;
#2977 = DIRECTION ( 'NONE',  ( -0.000000000000000000, -0.000000000000000000, 1.000000000000000000 ) ) ;
#2978 = ORIENTED_EDGE ( 'NONE', *, *, #506, .F. ) ;
#2979 = CARTESIAN_POINT ( 'NONE',  ( -51.19406879332065330, -13.71740939043347041, -10.50000000000000000 ) ) ;
#2980 = ORIENTED_EDGE ( 'NONE', *, *, #14625, .F. ) ;
#2981 = CARTESIAN_POINT ( 'NONE',  ( 9.716053034936797062, 106.5583837859906566, 19.49385781195229583 ) ) ;
#2982 = FACE_OUTER_BOUND ( 'NONE', #6132, .T. ) ;
#2983 = LINE ( 'NONE', #7684, #10246 ) ;
#2984 = DIRECTION ( 'NONE',  ( 1.000000000000000000, 0.000000000000000000, 0.000000000000000000 ) ) ;
#2985 = CARTESIAN_POINT ( 'NONE',  ( -65.64523757230321621, -68.01302780753330524, -8.000000000000000000 ) ) ;
#2986 = CARTESIAN_POINT ( 'NONE',  ( -11.08614924580848360, 94.35111528408442894, 18.49588680517285155 ) ) ;
#2987 = CIRCLE ( 'NONE', #9752, 0.2000000000000000944 ) ;
#2988 = VERTEX_POINT ( 'NONE', #14817 ) ;
#2989 = DIRECTION ( 'NONE',  ( 0.000000000000000000, 0.000000000000000000, -1.000000000000000000 ) ) ;
#2990 = DIRECTION ( 'NONE',  ( 0.000000000000000000, 0.000000000000000000, 1.000000000000000000 ) ) ;
#2991 = CIRCLE ( 'NONE', #1782, 10.00000000000000355 ) ;
#2992 = CARTESIAN_POINT ( 'NONE',  ( 3.999999999999998224, -0.8732470631450011123, -3.223155494240760977 ) ) ;
#2993 = EDGE_CURVE ( 'NONE', #5519, #12602, #14641, .T. ) ;
#2994 = ORIENTED_EDGE ( 'NONE', *, *, #14721, .F. ) ;
#2995 = VERTEX_POINT ( 'NONE', #5693 ) ;
#2996 = DIRECTION ( 'NONE',  ( 0.8660254037844379305, 0.5000000000000013323, 0.000000000000000000 ) ) ;
#2997 = ORIENTED_EDGE ( 'NONE', *, *, #3752, .F. ) ;
#2998 = DIRECTION ( 'NONE',  ( 0.000000000000000000, 0.000000000000000000, 1.000000000000000000 ) ) ;
#2999 = DIRECTION ( 'NONE',  ( -1.000000000000000000, 0.000000000000000000, 0.000000000000000000 ) ) ;
#3000 = ORIENTED_EDGE ( 'NONE', *, *, #6467, .F. ) ;
#3001 = CARTESIAN_POINT ( 'NONE',  ( 31.47058823529413374, 102.2673069760056563, -26.00000000000000000 ) ) ;
#3002 = FACE_OUTER_BOUND ( 'NONE', #10381, .T. ) ;
#3003 = DIRECTION ( 'NONE',  ( 1.000000000000000000, 0.000000000000000000, 0.000000000000000000 ) ) ;
#3004 = ORIENTED_EDGE ( 'NONE', *, *, #11647, .T. ) ;
#3005 = ORIENTED_EDGE ( 'NONE', *, *, #8971, .F. ) ;
#3006 = EDGE_LOOP ( 'NONE', ( #12500, #11613, #5941, #2708 ) ) ;
#3007 = CIRCLE ( 'NONE', #10524, 0.5000000000000038858 ) ;
#3008 = CARTESIAN_POINT ( 'NONE',  ( -52.54657765281192638, 6.917888187662934563, 8.000000000000000000 ) ) ;
#3009 = CARTESIAN_POINT ( 'NONE',  ( -49.00442420935969778, 30.80502811811250297, -10.50000000000000000 ) ) ;
#3010 = CIRCLE ( 'NONE', #1558, 60.50000000000000711 ) ;
#3011 = EDGE_CURVE ( 'NONE', #3028, #1282, #565, .T. ) ;
#3012 = DIRECTION ( 'NONE',  ( -0.000000000000000000, -0.000000000000000000, 1.000000000000000000 ) ) ;
#3013 = EDGE_CURVE ( 'NONE', #11582, #9151, #6359, .T. ) ;
#3015 = VERTEX_POINT ( 'NONE', #5061 ) ;
#3014 = EDGE_CURVE ( 'NONE', #2149, #297, #432, .T. ) ;
#3016 = ORIENTED_EDGE ( 'NONE', *, *, #12226, .F. ) ;
#3017 = EDGE_CURVE ( 'NONE', #3168, #5730, #2991, .T. ) ;
#3018 = ORIENTED_EDGE ( 'NONE', *, *, #7238, .F. ) ;
#3019 = AXIS2_PLACEMENT_3D ( 'NONE', #12124, #431, #5286 ) ;
#3020 = VECTOR ( 'NONE', #8405, 1000.000000000000000 ) ;
#3021 = EDGE_CURVE ( 'NONE', #2375, #14939, #11990, .T. ) ;
#3022 = CARTESIAN_POINT ( 'NONE',  ( 7.417888187663120192, 52.54657765281190507, -10.50000000000000000 ) ) ;
#3023 = EDGE_CURVE ( 'NONE', #12909, #2568, #5001, .T. ) ;
#3024 = AXIS2_PLACEMENT_3D ( 'NONE', #10373, #11675, #120 ) ;
#3025 = CARTESIAN_POINT ( 'NONE',  ( 0.000000000000000000, 0.000000000000000000, -10.50000000000000000 ) ) ;
#3026 =( NAMED_UNIT ( * ) PLANE_ANGLE_UNIT ( ) SI_UNIT ( $, .RADIAN. ) );
#3027 = DIRECTION ( 'NONE',  ( 0.000000000000000000, 0.000000000000000000, 1.000000000000000000 ) ) ;
#3028 = VERTEX_POINT ( 'NONE', #1502 ) ;
#3029 = ORIENTED_EDGE ( 'NONE', *, *, #12983, .T. ) ;
#3030 = LINE ( 'NONE', #4174, #7783 ) ;
#3031 = CARTESIAN_POINT ( 'NONE',  ( -32.45028783375101256, 101.9412720646926260, 14.06019896931749358 ) ) ;
#3032 = VERTEX_POINT ( 'NONE', #8623 ) ;
#3033 = DIRECTION ( 'NONE',  ( -0.000000000000000000, -0.000000000000000000, -1.000000000000000000 ) ) ;
#3034 = AXIS2_PLACEMENT_3D ( 'NONE', #8253, #14185, #10462 ) ;
#3035 = VECTOR ( 'NONE', #4382, 1000.000000000000000 ) ;
#3036 = CIRCLE ( 'NONE', #11536, 20.00000000000000000 ) ;
#3037 = ORIENTED_EDGE ( 'NONE', *, *, #1665, .F. ) ;
#3038 = B_SPLINE_CURVE_WITH_KNOTS ( 'NONE', 3,
 ( #5522, #13560, #10142, #10077 ),
 .UNSPECIFIED., .F., .F.,
 ( 4, 4 ),
 ( 0.000000000000000000, 0.001005167940839973807 ),
 .UNSPECIFIED. ) ;
#3039 = VERTEX_POINT ( 'NONE', #585 ) ;
#3040 = CARTESIAN_POINT ( 'NONE',  ( -29.95202887341199371, 96.45668229681565720, 12.61733007774791915 ) ) ;
#3041 = EDGE_CURVE ( 'NONE', #8922, #915, #11492, .T. ) ;
#3042 = FACE_OUTER_BOUND ( 'NONE', #3496, .T. ) ;
#3043 = PRODUCT_DEFINITION_CONTEXT ( 'detailed design', #6968, 'design' ) ;
#3044 = EDGE_CURVE ( 'NONE', #2764, #4760, #10509, .T. ) ;
#3045 = UNCERTAINTY_MEASURE_WITH_UNIT (LENGTH_MEASURE( 1.000000000000000082E-05 ), #9128, 'distance_accuracy_value', 'NONE');
#3046 = FACE_OUTER_BOUND ( 'NONE', #11594, .T. ) ;
#3047 = DIRECTION ( 'NONE',  ( 1.000000000000000000, 0.000000000000000000, 0.000000000000000000 ) ) ;
#3048 = CIRCLE ( 'NONE', #2798, 3.000000000000002665 ) ;
#3049 = CIRCLE ( 'NONE', #5223, 60.50000000000000000 ) ;
#3050 = DIRECTION ( 'NONE',  ( 1.000000000000000000, 0.000000000000000000, 0.000000000000000000 ) ) ;
#3051 = ORIENTED_EDGE ( 'NONE', *, *, #6748, .T. ) ;
#3052 = DIRECTION ( 'NONE',  ( -1.000000000000000000, 0.000000000000000000, -0.000000000000000000 ) ) ;
#3053 = AXIS2_PLACEMENT_3D ( 'NONE', #13485, #12283, #1869 ) ;
#3054 = DIRECTION ( 'NONE',  ( -0.000000000000000000, -0.000000000000000000, -1.000000000000000000 ) ) ;
#3055 = CARTESIAN_POINT ( 'NONE',  ( 4.211140560182194292, -2.431303136016555122, -3.745885042887437510 ) ) ;
#3056 = AXIS2_PLACEMENT_3D ( 'NONE', #3873, #11708, #8492 ) ;
#3057 = ORIENTED_EDGE ( 'NONE', *, *, #13026, .F. ) ;
#3058 =( LENGTH_UNIT ( ) NAMED_UNIT ( * ) SI_UNIT ( .MILLI., .METRE. ) );
#3059 = ADVANCED_FACE ( 'NONE', ( #5217 ), #7412, .T. ) ;
#3060 = DIRECTION ( 'NONE',  ( -0.000000000000000000, -0.000000000000000000, 1.000000000000000000 ) ) ;
#3061 = EDGE_CURVE ( 'NONE', #12145, #6775, #5658, .T. ) ;
#3062 = VERTEX_POINT ( 'NONE', #14254 ) ;
#3063 = DIRECTION ( 'NONE',  ( 0.000000000000000000, 0.000000000000000000, 1.000000000000000000 ) ) ;
#3064 = ORIENTED_EDGE ( 'NONE', *, *, #8857, .F. ) ;
#3065 = ORIENTED_EDGE ( 'NONE', *, *, #12364, .F. ) ;
#3066 = CARTESIAN_POINT ( 'NONE',  ( -12.50000000000000000, 100.2235002382176248, -15.00000000000000000 ) ) ;
#3067 = DIRECTION ( 'NONE',  ( 0.000000000000000000, 0.000000000000000000, -1.000000000000000000 ) ) ;
#3068 = CARTESIAN_POINT ( 'NONE',  ( 3.999999999999996447, 2.309401076758498039, -3.433295621305378020 ) ) ;
#3069 = CIRCLE ( 'NONE', #9111, 100.0000000000000000 ) ;
#3070 = DIRECTION ( 'NONE',  ( -0.000000000000000000, 1.000000000000000000, -0.000000000000000000 ) ) ;
#3071 = CYLINDRICAL_SURFACE ( 'NONE', #14400, 3.000000000000002665 ) ;
#3072 = EDGE_CURVE ( 'NONE', #9656, #6859, #4940, .T. ) ;
#3073 = ORIENTED_EDGE ( 'NONE', *, *, #3109, .T. ) ;
#3074 = CYLINDRICAL_SURFACE ( 'NONE', #1609, 3.000000000000002665 ) ;
#3075 = DIRECTION ( 'NONE',  ( 0.000000000000000000, 0.000000000000000000, -1.000000000000000000 ) ) ;
#3076 = CARTESIAN_POINT ( 'NONE',  ( 0.000000000000000000, 0.000000000000000000, 8.000000000000000000 ) ) ;
#3077 = VECTOR ( 'NONE', #8143, 1000.000000000000000 ) ;
#3078 = EDGE_CURVE ( 'NONE', #14649, #944, #9515, .T. ) ;
#3079 = ORIENTED_EDGE ( 'NONE', *, *, #6464, .T. ) ;
#3080 = CARTESIAN_POINT ( 'NONE',  ( -12.39897948556635754, 94.18739463280904545, 16.00000000000000000 ) ) ;
#3081 = ORIENTED_EDGE ( 'NONE', *, *, #11550, .T. ) ;
#3082 = FACE_OUTER_BOUND ( 'NONE', #11334, .T. ) ;
#3083 = DIRECTION ( 'NONE',  ( 1.000000000000000000, 0.000000000000000000, 0.000000000000000000 ) ) ;
#3084 = ORIENTED_EDGE ( 'NONE', *, *, #6039, .T. ) ;
#3085 = CARTESIAN_POINT ( 'NONE',  ( 0.000000000000000000, 0.000000000000000000, 8.000000000000000000 ) ) ;
#3086 = CARTESIAN_POINT ( 'NONE',  ( -100.0000000000000000, 0.000000000000000000, -13.00000000000000178 ) ) ;
#3087 = DIRECTION ( 'NONE',  ( 6.123233995736766036E-17, 0.000000000000000000, 1.000000000000000000 ) ) ;
#3088 = ORIENTED_EDGE ( 'NONE', *, *, #7200, .T. ) ;
#3089 = ORIENTED_EDGE ( 'NONE', *, *, #7585, .F. ) ;
#3090 = DIRECTION ( 'NONE',  ( 1.000000000000000000, 0.000000000000000000, 0.000000000000000000 ) ) ;
#3091 = CARTESIAN_POINT ( 'NONE',  ( 33.32958405265417667, 101.6044047647129958, 14.99207720203049199 ) ) ;
#3092 = LINE ( 'NONE', #9906, #9049 ) ;
#3093 = EDGE_LOOP ( 'NONE', ( #8891, #811 ) ) ;
#3094 = EDGE_LOOP ( 'NONE', ( #14388, #3409, #5176, #2342, #13518 ) ) ;
#3095 = ORIENTED_EDGE ( 'NONE', *, *, #7352, .T. ) ;
#3096 = ORIENTED_EDGE ( 'NONE', *, *, #14155, .F. ) ;
#3097 = CARTESIAN_POINT ( 'NONE',  ( 0.000000000000000000, 4.618802153517009401, -5.000000000000000888 ) ) ;
#3098 = EDGE_CURVE ( 'NONE', #4822, #13864, #14877, .T. ) ;
#3099 = DIRECTION ( 'NONE',  ( 1.000000000000000000, 0.000000000000000000, -0.000000000000000000 ) ) ;
#3100 = EDGE_CURVE ( 'NONE', #14147, #13178, #11832, .T. ) ;
#3101 = LINE ( 'NONE', #13733, #7179 ) ;
#3102 = EDGE_CURVE ( 'NONE', #7535, #5322, #5894, .T. ) ;
#3103 = CARTESIAN_POINT ( 'NONE',  ( 92.61631465359491244, 37.12029293941346708, 8.000000000000000000 ) ) ;
#3104 = CARTESIAN_POINT ( 'NONE',  ( -31.77701906416544730, 102.1706497334997863, 12.77113345645743969 ) ) ;
#3105 = EDGE_LOOP ( 'NONE', ( #1584, #2884, #7100, #9089, #538, #15005, #13987 ) ) ;
#3106 = CARTESIAN_POINT ( 'NONE',  ( 0.000000000000000000, 0.000000000000000000, -10.50000000000000000 ) ) ;
#3107 = ORIENTED_EDGE ( 'NONE', *, *, #4805, .F. ) ;
#3108 = ORIENTED_EDGE ( 'NONE', *, *, #9123, .F. ) ;
#3109 = EDGE_CURVE ( 'NONE', #6283, #8922, #4924, .T. ) ;
#3110 = ORIENTED_EDGE ( 'NONE', *, *, #7123, .F. ) ;
#3111 = FACE_OUTER_BOUND ( 'NONE', #643, .T. ) ;
#3112 = EDGE_CURVE ( 'NONE', #2908, #12963, #13194, .T. ) ;
#3113 = FACE_OUTER_BOUND ( 'NONE', #13889, .T. ) ;
#3114 = DIRECTION ( 'NONE',  ( -0.000000000000000000, -0.000000000000000000, 1.000000000000000000 ) ) ;
#3115 = DIRECTION ( 'NONE',  ( 0.000000000000000000, 0.000000000000000000, 1.000000000000000000 ) ) ;
#3116 = ADVANCED_FACE ( 'NONE', ( #5141 ), #6329, .T. ) ;
#3117 = EDGE_LOOP ( 'NONE', ( #2270, #1534, #3064, #9365 ) ) ;
#3118 = DIRECTION ( 'NONE',  ( -1.000000000000000000, 0.000000000000000000, 0.000000000000000000 ) ) ;
#3119 = ORIENTED_EDGE ( 'NONE', *, *, #5188, .T. ) ;
#3120 = VECTOR ( 'NONE', #9182, 1000.000000000000000 ) ;
#3121 = DIRECTION ( 'NONE',  ( 0.000000000000000000, 0.000000000000000000, -1.000000000000000000 ) ) ;
#3122 = CARTESIAN_POINT ( 'NONE',  ( 0.000000000000000000, 0.000000000000000000, -0.2800830152838856835 ) ) ;
#3123 = DIRECTION ( 'NONE',  ( 0.000000000000000000, 0.000000000000000000, 1.000000000000000000 ) ) ;
#3124 = ORIENTED_EDGE ( 'NONE', *, *, #6862, .F. ) ;
#3125 = CARTESIAN_POINT ( 'NONE',  ( 55.00000000000000000, -6.735557395310442615E-15, -13.00000000000000178 ) ) ;
#3126 = CARTESIAN_POINT ( 'NONE',  ( -12.50000000000000000, 106.2673515243510991, -15.00000000000000000 ) ) ;
#3127 = VERTEX_POINT ( 'NONE', #10677 ) ;
#3128 = B_SPLINE_CURVE_WITH_KNOTS ( 'NONE', 3,
 ( #9703, #10857, #456, #11942, #5026, #11791 ),
 .UNSPECIFIED., .F., .F.,
 ( 4, 2, 4 ),
 ( 0.002365888236227963858, 0.003551327329835074140, 0.004736766423442183988 ),
 .UNSPECIFIED. ) ;
#3129 = CARTESIAN_POINT ( 'NONE',  ( 46.63108361037843252, 56.43380494353993271, -10.50000000000000000 ) ) ;
#3130 = DIRECTION ( 'NONE',  ( 1.000000000000000000, 0.000000000000000000, 0.000000000000000000 ) ) ;
#3131 = CARTESIAN_POINT ( 'NONE',  ( -2.805705207896067144, 3.226868319750154868, -3.503898532754365025 ) ) ;
#3132 = CARTESIAN_POINT ( 'NONE',  ( 47.21331623427115431, 33.48561063518610581, 10.49999999999999822 ) ) ;
#3133 = B_SPLINE_CURVE_WITH_KNOTS ( 'NONE', 3,
 ( #11778, #1372, #5984, #10620, #4495 ),
 .UNSPECIFIED., .F., .F.,
 ( 4, 1, 4 ),
 ( 0.000000000000000000, 0.002309401076758505790, 0.004618802153517011580 ),
 .UNSPECIFIED. ) ;
#3134 = FACE_OUTER_BOUND ( 'NONE', #12510, .T. ) ;
#3135 = DIRECTION ( 'NONE',  ( -0.000000000000000000, -0.000000000000000000, -1.000000000000000000 ) ) ;
#3136 = CIRCLE ( 'NONE', #463, 2.649999999999985700 ) ;
#3137 = VERTEX_POINT ( 'NONE', #11909 ) ;
#3138 = CARTESIAN_POINT ( 'NONE',  ( 97.00000000000000000, -3.384287605079545030E-13, 8.000000000000000000 ) ) ;
#3139 = EDGE_CURVE ( 'NONE', #4446, #259, #1543, .T. ) ;
#3140 = ORIENTED_EDGE ( 'NONE', *, *, #6417, .T. ) ;
#3141 = ADVANCED_FACE ( 'NONE', ( #8849 ), #10019, .F. ) ;
#3142 = DIRECTION ( 'NONE',  ( 0.000000000000000000, 0.000000000000000000, 1.000000000000000000 ) ) ;
#3143 = CARTESIAN_POINT ( 'NONE',  ( 12.05137958362237960, 94.23255994477487718, -17.08976535968791310 ) ) ;
#3144 = ADVANCED_FACE ( 'NONE', ( #14554 ), #7555, .T. ) ;
#3145 = DIRECTION ( 'NONE',  ( -1.000000000000000000, 0.000000000000000000, 0.000000000000000000 ) ) ;
#3146 = FACE_OUTER_BOUND ( 'NONE', #4655, .T. ) ;
#3147 = ORIENTED_EDGE ( 'NONE', *, *, #14087, .T. ) ;
#3148 = ADVANCED_FACE ( 'NONE', ( #899 ), #14636, .F. ) ;
#3149 = DIRECTION ( 'NONE',  ( 0.000000000000000000, 0.000000000000000000, 1.000000000000000000 ) ) ;
#3150 = CIRCLE ( 'NONE', #11640, 22.00000000000000000 ) ;
#3151 = ORIENTED_EDGE ( 'NONE', *, *, #11980, .F. ) ;
#3152 = DIRECTION ( 'NONE',  ( 0.000000000000000000, 0.000000000000000000, -1.000000000000000000 ) ) ;
#3153 = DIRECTION ( 'NONE',  ( 1.000000000000000000, 0.000000000000000000, 0.000000000000000000 ) ) ;
#3154 = ORIENTED_EDGE ( 'NONE', *, *, #1066, .F. ) ;
#3155 = CARTESIAN_POINT ( 'NONE',  ( 11.46932393819253804, 106.3836852522821488, -18.05815993169796130 ) ) ;
#3156 = DIRECTION ( 'NONE',  ( 1.000000000000000000, 0.000000000000000000, 0.000000000000000000 ) ) ;
#3157 = ITEM_DEFINED_TRANSFORMATION ( 'NONE', 'NONE', #3389,  #5108 ) ;
#3158 = ORIENTED_EDGE ( 'NONE', *, *, #9090, .F. ) ;
#3159 = CIRCLE ( 'NONE', #6761, 63.00000000000000000 ) ;
#3160 = ORIENTED_EDGE ( 'NONE', *, *, #1928, .T. ) ;
#3161 = EDGE_CURVE ( 'NONE', #4530, #9110, #823, .T. ) ;
#3162 = CIRCLE ( 'NONE', #5091, 59.49999999999999289 ) ;
#3163 = DIRECTION ( 'NONE',  ( 1.000000000000000000, 0.000000000000000000, 0.000000000000000000 ) ) ;
#3164 = CARTESIAN_POINT ( 'NONE',  ( 34.09969740539978744, 101.2725728942521073, 15.50446122302712304 ) ) ;
#3165 = AXIS2_PLACEMENT_3D ( 'NONE', #5686, #3416, #8040 ) ;
#3166 = DIRECTION ( 'NONE',  ( -1.000000000000000000, 0.000000000000000000, 0.000000000000000000 ) ) ;
#3167 = EDGE_LOOP ( 'NONE', ( #7347, #9473 ) ) ;
#3168 = VERTEX_POINT ( 'NONE', #4158 ) ;
#3169 = ORIENTED_EDGE ( 'NONE', *, *, #5139, .F. ) ;
#3170 = DIRECTION ( 'NONE',  ( 0.000000000000000000, 0.000000000000000000, -1.000000000000000000 ) ) ;
#3171 = AXIS2_PLACEMENT_3D ( 'NONE', #1012, #4509, #2292 ) ;
#3172 = AXIS2_PLACEMENT_3D ( 'NONE', #10688, #3720, #8340 ) ;
#3173 = PLANE ( 'NONE',  #7579 ) ;
#3174 = FILL_AREA_STYLE ('',( #12438 ) ) ;
#3175 = CARTESIAN_POINT ( 'NONE',  ( -0.2790467552932217599, 96.58511096861892042, -10.50000000000000000 ) ) ;
#3176 = ORIENTED_EDGE ( 'NONE', *, *, #3014, .T. ) ;
#3177 = DIRECTION ( 'NONE',  ( 1.000000000000000000, 0.000000000000000000, 0.000000000000000000 ) ) ;
#3178 = DIRECTION ( 'NONE',  ( -1.000000000000000000, 0.000000000000000000, 0.000000000000000000 ) ) ;
#3179 = ORIENTED_EDGE ( 'NONE', *, *, #13517, .T. ) ;
#3180 = AXIS2_PLACEMENT_3D ( 'NONE', #6148, #5250, #2667 ) ;
#3181 = ORIENTED_EDGE ( 'NONE', *, *, #14610, .T. ) ;
#3182 = AXIS2_PLACEMENT_3D ( 'NONE', #10973, #8683, #575 ) ;
#3183 = AXIS2_PLACEMENT_3D ( 'NONE', #7484, #2725, #7342 ) ;
#3184 = VERTEX_POINT ( 'NONE', #5365 ) ;
#3185 = FACE_OUTER_BOUND ( 'NONE', #6867, .T. ) ;
#3186 = EDGE_CURVE ( 'NONE', #14403, #9441, #7101, .T. ) ;
#3187 = DIRECTION ( 'NONE',  ( 0.000000000000000000, 0.000000000000000000, 1.000000000000000000 ) ) ;
#3188 = CARTESIAN_POINT ( 'NONE',  ( -90.10640870805754332, -37.02125851216322872, 10.49999999999999822 ) ) ;
#3189 = CIRCLE ( 'NONE', #1737, 60.50000000000000000 ) ;
#3190 = DIRECTION ( 'NONE',  ( 0.000000000000000000, 0.000000000000000000, 1.000000000000000000 ) ) ;
#3191 = CARTESIAN_POINT ( 'NONE',  ( -24.98583958711379083, -30.74264578624812927, -28.00000000000000000 ) ) ;
#3192 = LINE ( 'NONE', #9861, #11146 ) ;
#3193 = VECTOR ( 'NONE', #14768, 1000.000000000000000 ) ;
#3194 = ORIENTED_EDGE ( 'NONE', *, *, #4743, .F. ) ;
#3195 = FACE_OUTER_BOUND ( 'NONE', #2617, .T. ) ;
#3196 = CARTESIAN_POINT ( 'NONE',  ( 12.28299983316190946, 61.79111512501306436, 16.56818193787249527 ) ) ;
#3197 = CARTESIAN_POINT ( 'NONE',  ( 2.805705207896068920, -3.226868319750169078, -3.503898532754369022 ) ) ;
#3198 = CIRCLE ( 'NONE', #3932, 3.000000000000002665 ) ;
#3199 = VERTEX_POINT ( 'NONE', #6639 ) ;
#3200 = DIRECTION ( 'NONE',  ( 1.224646799147353207E-16, 1.000000000000000000, 0.000000000000000000 ) ) ;
#3201 = EDGE_CURVE ( 'NONE', #13408, #2119, #12945, .T. ) ;
#3202 = EDGE_CURVE ( 'NONE', #13490, #4514, #3092, .T. ) ;
#3203 = EDGE_LOOP ( 'NONE', ( #6037, #1959, #11785, #2373, #6650, #6904, #11054, #14458, #6640 ) ) ;
#3204 = CARTESIAN_POINT ( 'NONE',  ( 2.000000000000008882, -3.464101615137750390, 0.000000000000000000 ) ) ;
#3205 = AXIS2_PLACEMENT_3D ( 'NONE', #2570, #14112, #3636 ) ;
#3206 = ORIENTED_EDGE ( 'NONE', *, *, #2258, .F. ) ;
#3207 = DIRECTION ( 'NONE',  ( 0.000000000000000000, 0.000000000000000000, 1.000000000000000000 ) ) ;
#3208 = DIRECTION ( 'NONE',  ( 0.000000000000000000, 0.000000000000000000, 1.000000000000000000 ) ) ;
#3209 = CARTESIAN_POINT ( 'NONE',  ( 2.449293598294700991E-16, -97.00000000000000000, -8.000000000000000000 ) ) ;
#3210 = DIRECTION ( 'NONE',  ( 1.000000000000000000, 0.000000000000000000, 0.000000000000000000 ) ) ;
#3211 = CARTESIAN_POINT ( 'NONE',  ( -30.80502811811232888, -49.00442420935981147, 10.49999999999999822 ) ) ;
#3212 = VECTOR ( 'NONE', #13025, 1000.000000000000000 ) ;
#3213 = FACE_BOUND ( 'NONE', #4830, .T. ) ;
#3214 = DIRECTION ( 'NONE',  ( 0.000000000000000000, 0.000000000000000000, 1.000000000000000000 ) ) ;
#3215 = ORIENTED_EDGE ( 'NONE', *, *, #2407, .F. ) ;
#3216 = CIRCLE ( 'NONE', #5637, 52.50000000000000711 ) ;
#3217 = DIRECTION ( 'NONE',  ( 0.000000000000000000, 0.000000000000000000, 1.000000000000000000 ) ) ;
#3218 = DIRECTION ( 'NONE',  ( -1.000000000000000000, 0.000000000000000000, 0.000000000000000000 ) ) ;
#3219 = LINE ( 'NONE', #1783, #9026 ) ;
#3220 = CARTESIAN_POINT ( 'NONE',  ( -3.492805317593278058, 46.55633131742322917, -10.50000000000000000 ) ) ;
#3221 = AXIS2_PLACEMENT_3D ( 'NONE', #4064, #12335, #3145 ) ;
#3222 = ORIENTED_EDGE ( 'NONE', *, *, #10093, .F. ) ;
#3223 = CARTESIAN_POINT ( 'NONE',  ( -56.43380494354004639, -12.86891638962099549, -10.50000000000000000 ) ) ;
#3224 = ORIENTED_EDGE ( 'NONE', *, *, #3759, .F. ) ;
#3225 = EDGE_CURVE ( 'NONE', #9151, #5320, #10274, .T. ) ;
#3226 = PLANE ( 'NONE',  #3270 ) ;
#3227 = DIRECTION ( 'NONE',  ( 0.000000000000000000, 0.000000000000000000, -1.000000000000000000 ) ) ;
#3228 = ORIENTED_EDGE ( 'NONE', *, *, #8429, .T. ) ;
#3229 = AXIS2_PLACEMENT_3D ( 'NONE', #7795, #14567, #13421 ) ;
#3230 = EDGE_CURVE ( 'NONE', #9159, #12354, #6712, .T. ) ;
#3231 = CARTESIAN_POINT ( 'NONE',  ( 52.50000000000000711, -6.429395695523604744E-15, -13.00000000000000178 ) ) ;
#3232 = DIRECTION ( 'NONE',  ( 1.000000000000000000, 0.000000000000000000, 0.000000000000000000 ) ) ;
#3233 = ORIENTED_EDGE ( 'NONE', *, *, #11476, .F. ) ;
#3234 = ORIENTED_EDGE ( 'NONE', *, *, #979, .F. ) ;
#3235 = ADVANCED_FACE ( 'NONE', ( #13333 ), #4239, .T. ) ;
#3236 = DIRECTION ( 'NONE',  ( 1.000000000000000000, 0.000000000000000000, 0.000000000000000000 ) ) ;
#3237 = CARTESIAN_POINT ( 'NONE',  ( -37.12029293941250074, 89.61631465359532456, -13.00000000000000178 ) ) ;
#3238 = DIRECTION ( 'NONE',  ( -0.000000000000000000, -0.000000000000000000, -1.000000000000000000 ) ) ;
#3239 = ORIENTED_EDGE ( 'NONE', *, *, #3299, .F. ) ;
#3240 = CIRCLE ( 'NONE', #6365, 63.00000000000000000 ) ;
#3241 = ORIENTED_EDGE ( 'NONE', *, *, #7025, .F. ) ;
#3242 = EDGE_CURVE ( 'NONE', #13289, #337, #11214, .T. ) ;
#3243 = ORIENTED_EDGE ( 'NONE', *, *, #7112, .F. ) ;
#3244 = AXIS2_PLACEMENT_3D ( 'NONE', #1424, #6033, #2634 ) ;
#3245 = EDGE_CURVE ( 'NONE', #5022, #11082, #2508, .T. ) ;
#3246 = CARTESIAN_POINT ( 'NONE',  ( 9.706953719245472456, 57.06275842387054098, -13.00000000000000178 ) ) ;
#3247 = CARTESIAN_POINT ( 'NONE',  ( 9.706953719245472456, 57.06275842387054098, 8.000000000000000000 ) ) ;
#3248 = CARTESIAN_POINT ( 'NONE',  ( 37.12029293941315444, -89.61631465359504034, -13.00000000000000178 ) ) ;
#3249 = CARTESIAN_POINT ( 'NONE',  ( -50.69406879332065330, -13.71740939043347041, -13.00000000000000178 ) ) ;
#3250 = CIRCLE ( 'NONE', #4713, 0.5000000000000004441 ) ;
#3251 = AXIS2_PLACEMENT_3D ( 'NONE', #11189, #5336, #790 ) ;
#3252 = CYLINDRICAL_SURFACE ( 'NONE', #3673, 3.000000000000002665 ) ;
#3253 = CARTESIAN_POINT ( 'NONE',  ( 3.999999999999996447, -2.309401076758518911, -3.433295621305385126 ) ) ;
#3254 = ORIENTED_EDGE ( 'NONE', *, *, #13997, .F. ) ;
#3255 = EDGE_CURVE ( 'NONE', #4753, #1381, #12910, .T. ) ;
#3256 = CARTESIAN_POINT ( 'NONE',  ( -56.43380494354004639, -12.86891638962099549, -13.00000000000000178 ) ) ;
#3257 = ORIENTED_EDGE ( 'NONE', *, *, #11318, .F. ) ;
#3258 = ORIENTED_EDGE ( 'NONE', *, *, #73, .F. ) ;
#3259 = CARTESIAN_POINT ( 'NONE',  ( -4.154094228333540251, 2.398367420968064323, -3.721909803043256915 ) ) ;
#3260 = VECTOR ( 'NONE', #3652, 1000.000000000000114 ) ;
#3261 = AXIS2_PLACEMENT_3D ( 'NONE', #11841, #9683, #9612 ) ;
#3262 = AXIS2_PLACEMENT_3D ( 'NONE', #13302, #271, #14449 ) ;
#3263 = EDGE_LOOP ( 'NONE', ( #4692, #7429, #3241, #13964, #12511, #9372 ) ) ;
#3264 = DIRECTION ( 'NONE',  ( 1.000000000000000000, 0.000000000000000000, 0.000000000000000000 ) ) ;
#3265 = CARTESIAN_POINT ( 'NONE',  ( 20.00000000000000000, 0.000000000000000000, -43.49999999999998579 ) ) ;
#3266 = FACE_OUTER_BOUND ( 'NONE', #1812, .T. ) ;
#3267 = AXIS2_PLACEMENT_3D ( 'NONE', #5221, #8904, #1580 ) ;
#3268 = DIRECTION ( 'NONE',  ( 1.000000000000000000, 0.000000000000000000, 0.000000000000000000 ) ) ;
#3269 = ORIENTED_EDGE ( 'NONE', *, *, #12432, .T. ) ;
#3270 = AXIS2_PLACEMENT_3D ( 'NONE', #7844, #10125, #806 ) ;
#3271 = CONICAL_SURFACE ( 'NONE', #13213, 4.000000000000000000, 0.8911886515913786111 ) ;
#3272 = DIRECTION ( 'NONE',  ( 1.000000000000000000, 0.000000000000000000, 0.000000000000000000 ) ) ;
#3273 = CIRCLE ( 'NONE', #12252, 53.55662432702593634 ) ;
#3274 = ORIENTED_EDGE ( 'NONE', *, *, #5017, .F. ) ;
#3275 = CARTESIAN_POINT ( 'NONE',  ( 12.39897948556635754, 61.76783392443436327, 16.00000000000000000 ) ) ;
#3276 = CARTESIAN_POINT ( 'NONE',  ( 18.52941176470587692, 60.21346111671358159, 31.00000000000000000 ) ) ;
#3277 = ORIENTED_EDGE ( 'NONE', *, *, #5289, .F. ) ;
#3278 = DIRECTION ( 'NONE',  ( 1.000000000000000000, 0.000000000000000000, 0.000000000000000000 ) ) ;
#3279 = CIRCLE ( 'NONE', #10071, 3.000000000000002665 ) ;
#3280 = CARTESIAN_POINT ( 'NONE',  ( 29.73684566822694464, 96.52317875358639299, 11.65491793965443357 ) ) ;
#3281 = AXIS2_PLACEMENT_3D ( 'NONE', #14701, #4447, #9058 ) ;
#3282 = DIRECTION ( 'NONE',  ( 1.000000000000000000, 0.000000000000000000, 0.000000000000000000 ) ) ;
#3283 = AXIS2_PLACEMENT_3D ( 'NONE', #2960, #9105, #8942 ) ;
#3284 = CYLINDRICAL_SURFACE ( 'NONE', #11291, 2.649999999999992806 ) ;
#3285 = CARTESIAN_POINT ( 'NONE',  ( -11.26223186129995391, 106.4059016791561447, 18.30934846123060922 ) ) ;
#3286 = FACE_OUTER_BOUND ( 'NONE', #11438, .T. ) ;
#3287 = EDGE_CURVE ( 'NONE', #5421, #7249, #4918, .T. ) ;
#3288 = LINE ( 'NONE', #7909, #3626 ) ;
#3289 = EDGE_CURVE ( 'NONE', #4561, #3819, #14859, .T. ) ;
#3290 = CARTESIAN_POINT ( 'NONE',  ( -44.89637028918153305, 0.000000000000000000, -25.50000000000000355 ) ) ;
#3291 = EDGE_CURVE ( 'NONE', #11078, #8255, #13161, .T. ) ;
#3292 = EDGE_CURVE ( 'NONE', #6509, #203, #10238, .T. ) ;
#3293 = CARTESIAN_POINT ( 'NONE',  ( 26.01438936481372721, 47.21331623427104063, -10.50000000000000000 ) ) ;
#3294 = CIRCLE ( 'NONE', #5712, 59.50000000000000000 ) ;
#3295 = ORIENTED_EDGE ( 'NONE', *, *, #11069, .F. ) ;
#3296 = DIRECTION ( 'NONE',  ( 0.000000000000000000, 0.000000000000000000, 1.000000000000000000 ) ) ;
#3297 = DIRECTION ( 'NONE',  ( 0.000000000000000000, 0.000000000000000000, 1.000000000000000000 ) ) ;
#3298 = FACE_OUTER_BOUND ( 'NONE', #9987, .T. ) ;
#3299 = EDGE_CURVE ( 'NONE', #12763, #6631, #9273, .T. ) ;
#3300 = DIRECTION ( 'NONE',  ( 0.000000000000000000, 0.000000000000000000, 1.000000000000000000 ) ) ;
#3301 = VERTEX_POINT ( 'NONE', #10437 ) ;
#3302 = CIRCLE ( 'NONE', #1599, 3.000000000000002665 ) ;
#3303 = CARTESIAN_POINT ( 'NONE',  ( -1.287237434361998778, -3.875615274276856592, -3.430618716626631759 ) ) ;
#3304 = CONICAL_SURFACE ( 'NONE', #4031, 2.041999999999999815, 1.047197551196591858 ) ;
#3305 = ORIENTED_EDGE ( 'NONE', *, *, #11458, .T. ) ;
#3306 = DIRECTION ( 'NONE',  ( 0.000000000000000000, 0.000000000000000000, -1.000000000000000000 ) ) ;
#3307 = CARTESIAN_POINT ( 'NONE',  ( 37.12029293941315444, -89.61631465359504034, -8.000000000000000000 ) ) ;
#3308 = CARTESIAN_POINT ( 'NONE',  ( 9.706953719245472456, 57.06275842387054098, -8.000000000000000000 ) ) ;
#3309 = LINE ( 'NONE', #7928, #13193 ) ;
#3310 = ORIENTED_EDGE ( 'NONE', *, *, #5017, .T. ) ;
#3311 = EDGE_CURVE ( 'NONE', #8664, #14518, #14369, .T. ) ;
#3312 = ORIENTED_EDGE ( 'NONE', *, *, #11427, .F. ) ;
#3313 = ORIENTED_EDGE ( 'NONE', *, *, #13919, .T. ) ;
#3314 = AXIS2_PLACEMENT_3D ( 'NONE', #1697, #5195, #9885 ) ;
#3315 = CYLINDRICAL_SURFACE ( 'NONE', #5719, 0.5000000000000022204 ) ;
#3316 = CARTESIAN_POINT ( 'NONE',  ( 35.79345569434273244, 100.4135791079097544, 15.99999999999999645 ) ) ;
#3317 = CARTESIAN_POINT ( 'NONE',  ( 2.449293598294700991E-16, -97.00000000000000000, -8.000000000000000000 ) ) ;
#3318 = ORIENTED_EDGE ( 'NONE', *, *, #9787, .F. ) ;
#3319 = ORIENTED_EDGE ( 'NONE', *, *, #4805, .T. ) ;
#3320 = VECTOR ( 'NONE', #6649, 1000.000000000000000 ) ;
#3321 = EDGE_LOOP ( 'NONE', ( #10041, #10010, #996, #6082 ) ) ;
#3322 = AXIS2_PLACEMENT_3D ( 'NONE', #10118, #9277, #13929 ) ;
#3323 = DIRECTION ( 'NONE',  ( 1.000000000000000000, 0.000000000000000000, 0.000000000000000000 ) ) ;
#3324 = CARTESIAN_POINT ( 'NONE',  ( 47.21331623427115431, 33.48561063518610581, 10.49999999999999822 ) ) ;
#3325 = DIRECTION ( 'NONE',  ( -0.000000000000000000, -0.000000000000000000, 1.000000000000000000 ) ) ;
#3326 = CYLINDRICAL_SURFACE ( 'NONE', #1861, 59.50000000000000000 ) ;
#3327 = CARTESIAN_POINT ( 'NONE',  ( -12.39897948556635754, 61.76783392443436327, -16.00000000000000000 ) ) ;
#3328 = ORIENTED_EDGE ( 'NONE', *, *, #4719, .F. ) ;
#3329 = DIRECTION ( 'NONE',  ( 1.000000000000000000, 0.000000000000000000, 0.000000000000000000 ) ) ;
#3331 = EDGE_CURVE ( 'NONE', #5203, #337, #8083, .T. ) ;
#3330 = DIRECTION ( 'NONE',  ( 0.000000000000000000, 0.000000000000000000, 1.000000000000000000 ) ) ;
#3332 = EDGE_CURVE ( 'NONE', #12052, #6195, #9150, .T. ) ;
#3333 = ORIENTED_EDGE ( 'NONE', *, *, #12594, .T. ) ;
#3334 = ORIENTED_EDGE ( 'NONE', *, *, #4129, .F. ) ;
#3335 = CARTESIAN_POINT ( 'NONE',  ( 0.000000000000000000, 0.000000000000000000, -5.000000000000000888 ) ) ;
#3336 = CYLINDRICAL_SURFACE ( 'NONE', #3909, 7.500000000000001776 ) ;
#3337 = ADVANCED_FACE ( 'NONE', ( #1183 ), #6939, .F. ) ;
#3338 = CARTESIAN_POINT ( 'NONE',  ( -25.00000000000000000, 81.24038404635962252, -23.50000000000000000 ) ) ;
#3339 = DIRECTION ( 'NONE',  ( 1.000000000000000000, 0.000000000000000000, 0.000000000000000000 ) ) ;
#3340 = DIRECTION ( 'NONE',  ( -1.000000000000000000, 9.175396897728567444E-16, 0.000000000000000000 ) ) ;
#3341 = DIRECTION ( 'NONE',  ( 0.000000000000000000, 0.000000000000000000, -1.000000000000000000 ) ) ;
#3342 = EDGE_LOOP ( 'NONE', ( #8519, #2544, #13031, #3005, #11209, #8955 ) ) ;
#3343 = FACE_OUTER_BOUND ( 'NONE', #2177, .T. ) ;
#3344 = ORIENTED_EDGE ( 'NONE', *, *, #9352, .T. ) ;
#3345 = EDGE_CURVE ( 'NONE', #3039, #11882, #7813, .T. ) ;
#3346 = CARTESIAN_POINT ( 'NONE',  ( -42.04772703543551415, -32.26435573746212526, -8.000000000000000000 ) ) ;
#3347 = DIRECTION ( 'NONE',  ( 0.000000000000000000, 0.000000000000000000, 1.000000000000000000 ) ) ;
#3348 = ORIENTED_EDGE ( 'NONE', *, *, #2296, .T. ) ;
#3349 = CARTESIAN_POINT ( 'NONE',  ( 89.89283556784508278, -37.53686968382275779, -13.00000000000000178 ) ) ;
#3350 = ORIENTED_EDGE ( 'NONE', *, *, #4500, .F. ) ;
#3351 = CARTESIAN_POINT ( 'NONE',  ( 29.70588235294119528, 96.53269163155674448, 11.33021710499463985 ) ) ;
#3352 = AXIS2_PLACEMENT_3D ( 'NONE', #7097, #13891, #2562 ) ;
#3353 = DIRECTION ( 'NONE',  ( 0.000000000000000000, 0.000000000000000000, -1.000000000000000000 ) ) ;
#3354 = FACE_OUTER_BOUND ( 'NONE', #5895, .T. ) ;
#3355 = CARTESIAN_POINT ( 'NONE',  ( -9.260566377415146988, 106.5986160369160416, 19.68264575353695989 ) ) ;
#3356 = CYLINDRICAL_SURFACE ( 'NONE', #6593, 75.00000000000001421 ) ;
#3357 = CARTESIAN_POINT ( 'NONE',  ( -3.999999999999998224, -1.680117682357869624, -3.316611593219199072 ) ) ;
#3358 = CARTESIAN_POINT ( 'NONE',  ( 0.000000000000000000, 0.000000000000000000, -45.50000000000000000 ) ) ;
#3359 = ORIENTED_EDGE ( 'NONE', *, *, #6971, .F. ) ;
#3360 = DIRECTION ( 'NONE',  ( -1.000000000000000000, 0.000000000000000000, 0.000000000000000000 ) ) ;
#3361 = CARTESIAN_POINT ( 'NONE',  ( 33.48561063518626923, -47.21331623427104063, 10.49999999999999822 ) ) ;
#3362 = DIRECTION ( 'NONE',  ( 0.000000000000000000, 0.000000000000000000, 1.000000000000000000 ) ) ;
#3363 = CARTESIAN_POINT ( 'NONE',  ( -42.04772703543551415, -32.26435573746212526, -10.50000000000000000 ) ) ;
#3364 = ORIENTED_EDGE ( 'NONE', *, *, #11977, .T. ) ;
#3365 = EDGE_CURVE ( 'NONE', #2335, #13021, #13394, .T. ) ;
#3366 = DIRECTION ( 'NONE',  ( -0.2941176470588243164, -0.9557692240748185686, -0.000000000000000000 ) ) ;
#3367 = EDGE_CURVE ( 'NONE', #967, #3376, #13898, .T. ) ;
#3368 = ORIENTED_EDGE ( 'NONE', *, *, #7369, .F. ) ;
#3369 = FACE_OUTER_BOUND ( 'NONE', #4376, .T. ) ;
#3370 = FACE_OUTER_BOUND ( 'NONE', #11300, .T. ) ;
#3371 = AXIS2_PLACEMENT_3D ( 'NONE', #4104, #3118, #1896 ) ;
#3372 = DIRECTION ( 'NONE',  ( 1.000000000000000000, 0.000000000000000000, 0.000000000000000000 ) ) ;
#3373 = DIRECTION ( 'NONE',  ( -0.000000000000000000, -0.000000000000000000, 1.000000000000000000 ) ) ;
#3374 = ORIENTED_EDGE ( 'NONE', *, *, #13577, .F. ) ;
#3375 = ORIENTED_EDGE ( 'NONE', *, *, #14454, .F. ) ;
#3376 = VERTEX_POINT ( 'NONE', #6781 ) ;
#3377 = ORIENTED_EDGE ( 'NONE', *, *, #12523, .T. ) ;
#3378 = CARTESIAN_POINT ( 'NONE',  ( -15.11621636258860946, 32.12188890498260463, -16.00000000000000000 ) ) ;
#3379 = AXIS2_PLACEMENT_3D ( 'NONE', #497, #11129, #7403 ) ;
#3380 = DIRECTION ( 'NONE',  ( -1.000000000000000000, 0.000000000000000000, 0.000000000000000000 ) ) ;
#3381 = DIRECTION ( 'NONE',  ( 1.000000000000000000, 0.000000000000000000, 0.000000000000000000 ) ) ;
#3382 = ORIENTED_EDGE ( 'NONE', *, *, #1535, .F. ) ;
#3383 = AXIS2_PLACEMENT_3D ( 'NONE', #14740, #6358, #14590 ) ;
#3384 = ORIENTED_EDGE ( 'NONE', *, *, #8246, .T. ) ;
#3385 = EDGE_CURVE ( 'NONE', #4050, #13764, #1336, .T. ) ;
#3386 = EDGE_CURVE ( 'NONE', #10213, #2325, #4674, .T. ) ;
#3387 = ORIENTED_EDGE ( 'NONE', *, *, #7926, .F. ) ;
#3388 = CARTESIAN_POINT ( 'NONE',  ( 9.448652591187071792, 74.40292581525912397, 19.61336856585178623 ) ) ;
#3389 = AXIS2_PLACEMENT_3D ( 'NONE', #1348, #1931, #3003 ) ;
#3390 = CIRCLE ( 'NONE', #13096, 4.999999999999995559 ) ;
#3391 = DIRECTION ( 'NONE',  ( -0.000000000000000000, -0.000000000000000000, 1.000000000000000000 ) ) ;
#3392 = CARTESIAN_POINT ( 'NONE',  ( 0.000000000000000000, 0.000000000000000000, -23.50000000000000000 ) ) ;
#3393 =( REPRESENTATION_RELATIONSHIP ('NONE','NONE', #12187, #12767 ) REPRESENTATION_RELATIONSHIP_WITH_TRANSFORMATION ( #4733 )SHAPE_REPRESENTATION_RELATIONSHIP( ) );
#3394 = AXIS2_PLACEMENT_3D ( 'NONE', #11038, #5190, #13017 ) ;
#3395 = LINE ( 'NONE', #3700, #14697 ) ;
#3396 = AXIS2_PLACEMENT_3D ( 'NONE', #8894, #1843, #13461 ) ;
#3397 = ORIENTED_EDGE ( 'NONE', *, *, #2435, .T. ) ;
#3398 = CARTESIAN_POINT ( 'NONE',  ( 0.000000000000000000, 0.000000000000000000, 10.50000000000000000 ) ) ;
#3399 = ORIENTED_EDGE ( 'NONE', *, *, #2956, .F. ) ;
#3400 = CIRCLE ( 'NONE', #3891, 60.50000000000000000 ) ;
#3401 = DIRECTION ( 'NONE',  ( -0.000000000000000000, -0.000000000000000000, -1.000000000000000000 ) ) ;
#3402 = DIRECTION ( 'NONE',  ( -1.000000000000000000, 0.000000000000000000, 0.000000000000000000 ) ) ;
#3403 = ORIENTED_EDGE ( 'NONE', *, *, #6611, .F. ) ;
#3404 = AXIS2_PLACEMENT_3D ( 'NONE', #2979, #9037, #5553 ) ;
#3405 = EDGE_LOOP ( 'NONE', ( #10883, #13151, #4480, #3749, #11608, #2485, #11173, #1742, #540, #8841 ) ) ;
#3406 = DIRECTION ( 'NONE',  ( 1.000000000000000000, 0.000000000000000000, -0.000000000000000000 ) ) ;
#3407 = AXIS2_PLACEMENT_3D ( 'NONE', #5629, #6530, #11188 ) ;
#3408 = ORIENTED_EDGE ( 'NONE', *, *, #2376, .F. ) ;
#3409 = ORIENTED_EDGE ( 'NONE', *, *, #7532, .T. ) ;
#3410 = DIRECTION ( 'NONE',  ( -0.000000000000000000, -0.000000000000000000, -1.000000000000000000 ) ) ;
#3411 = EDGE_CURVE ( 'NONE', #10761, #4919, #7563, .T. ) ;
#3412 = CARTESIAN_POINT ( 'NONE',  ( 45.91029614918936375, -26.00011991137331790, 10.49999999999999822 ) ) ;
#3413 = EDGE_CURVE ( 'NONE', #3032, #5002, #2450, .T. ) ;
#3414 = EDGE_CURVE ( 'NONE', #5837, #5604, #6590, .T. ) ;
#3415 = CARTESIAN_POINT ( 'NONE',  ( -2.000000000000008882, 3.464101615137750390, 0.000000000000000000 ) ) ;
#3416 = DIRECTION ( 'NONE',  ( 0.000000000000000000, 0.8660254037844381525, -0.5000000000000008882 ) ) ;
#3417 = AXIS2_PLACEMENT_3D ( 'NONE', #6443, #7735, #11328 ) ;
#3418 = ORIENTED_EDGE ( 'NONE', *, *, #14716, .F. ) ;
#3419 = CIRCLE ( 'NONE', #6546, 3.000000000000002665 ) ;
#3420 = CARTESIAN_POINT ( 'NONE',  ( 27.94117647058824616, 90.79807628710781842, 16.00000000000000000 ) ) ;
#3421 = EDGE_LOOP ( 'NONE', ( #1119, #1872, #10794, #12340, #4213, #3702, #7733, #6997, #10903, #14424, #7046 ) ) ;
#3422 = AXIS2_PLACEMENT_3D ( 'NONE', #9189, #11411, #5848 ) ;
#3423 = AXIS2_PLACEMENT_3D ( 'NONE', #3994, #10968, #569 ) ;
#3424 = ADVANCED_FACE ( 'NONE', ( #13872 ), #7934, .T. ) ;
#3425 = CARTESIAN_POINT ( 'NONE',  ( 0.000000000000000000, 0.000000000000000000, -8.000000000000000000 ) ) ;
#3426 = ORIENTED_EDGE ( 'NONE', *, *, #1273, .T. ) ;
#3427 = CARTESIAN_POINT ( 'NONE',  ( 25.00000000000000000, 81.24038404635960831, 16.00000000000000000 ) ) ;
#3428 = ORIENTED_EDGE ( 'NONE', *, *, #12098, .T. ) ;
#3429 = AXIS2_PLACEMENT_3D ( 'NONE', #11606, #12742, #13652 ) ;
#3430 = DIRECTION ( 'NONE',  ( -0.000000000000000000, -0.000000000000000000, 1.000000000000000000 ) ) ;
#3431 = EDGE_LOOP ( 'NONE', ( #14921, #4444, #7666, #7971 ) ) ;
#3432 = CARTESIAN_POINT ( 'NONE',  ( 0.6920835326022575229, 4.454600218803879130, -3.597382984111580306 ) ) ;
#3433 = VECTOR ( 'NONE', #8460, 1000.000000000000000 ) ;
#3434 = EDGE_CURVE ( 'NONE', #3819, #7980, #3463, .T. ) ;
#3435 = ADVANCED_FACE ( 'NONE', ( #2163 ), #11445, .F. ) ;
#3436 = CIRCLE ( 'NONE', #13612, 68.00000000000000000 ) ;
#3437 = DIRECTION ( 'NONE',  ( 1.000000000000000000, 0.000000000000000000, 0.000000000000000000 ) ) ;
#3438 = CARTESIAN_POINT ( 'NONE',  ( 52.36539807335608288, -6.451868917687384020, -10.50000000000000000 ) ) ;
#3439 = DIRECTION ( 'NONE',  ( 0.000000000000000000, 0.000000000000000000, 1.000000000000000000 ) ) ;
#3440 = DIRECTION ( 'NONE',  ( -1.000000000000000000, 0.000000000000000000, 0.000000000000000000 ) ) ;
#3441 = CARTESIAN_POINT ( 'NONE',  ( -26.49999999999971578, -45.89934640057541060, -10.50000000000000000 ) ) ;
#3442 = CIRCLE ( 'NONE', #8287, 50.00000000000000000 ) ;
#3443 = ORIENTED_EDGE ( 'NONE', *, *, #13676, .T. ) ;
#3444 = CARTESIAN_POINT ( 'NONE',  ( 5.200000000000006395, 0.000000000000000000, 2.775557561562891351E-14 ) ) ;
#3445 = CARTESIAN_POINT ( 'NONE',  ( 0.000000000000000000, 0.000000000000000000, -10.50000000000000000 ) ) ;
#3446 = CIRCLE ( 'NONE', #13910, 3.000000000000002665 ) ;
#3447 = AXIS2_PLACEMENT_3D ( 'NONE', #12453, #9249, #10393 ) ;
#3448 = CARTESIAN_POINT ( 'NONE',  ( 50.84834283436990177, 14.07862063237912054, -10.50000000000000000 ) ) ;
#3449 = DIRECTION ( 'NONE',  ( 1.000000000000000000, 0.000000000000000000, 0.000000000000000000 ) ) ;
#3450 = VERTEX_POINT ( 'NONE', #5662 ) ;
#3451 = DIRECTION ( 'NONE',  ( 0.000000000000000000, 0.000000000000000000, 1.000000000000000000 ) ) ;
#3452 = ORIENTED_EDGE ( 'NONE', *, *, #4242, .T. ) ;
#3453 = MECHANICAL_DESIGN_GEOMETRIC_PRESENTATION_REPRESENTATION (  '', ( #8495 ), #12388 ) ;
#3454 = DIRECTION ( 'NONE',  ( -1.000000000000000000, 0.000000000000000000, 0.000000000000000000 ) ) ;
#3455 = CARTESIAN_POINT ( 'NONE',  ( -3.999999999999996447, 0.9868501483902569760, -0.09357334158579228012 ) ) ;
#3456 = LINE ( 'NONE', #12792, #1255 ) ;
#3457 = CIRCLE ( 'NONE', #7317, 60.50000000000000711 ) ;
#3458 = CARTESIAN_POINT ( 'NONE',  ( -56.43380494354004639, -12.86891638962099549, 10.49999999999999822 ) ) ;
#3459 = ORIENTED_EDGE ( 'NONE', *, *, #15021, .T. ) ;
#3460 = CARTESIAN_POINT ( 'NONE',  ( 97.00000000000000000, -3.384287605079545030E-13, -13.00000000000000178 ) ) ;
#3461 = LINE ( 'NONE', #3612, #12236 ) ;
#3462 = CIRCLE ( 'NONE', #11956, 0.5000000000000022204 ) ;
#3463 = LINE ( 'NONE', #13950, #5873 ) ;
#3464 = VERTEX_POINT ( 'NONE', #1260 ) ;
#3465 = AXIS2_PLACEMENT_3D ( 'NONE', #12621, #3439, #10486 ) ;
#3466 = ORIENTED_EDGE ( 'NONE', *, *, #4698, .F. ) ;
#3467 = EDGE_LOOP ( 'NONE', ( #653, #3348, #4904, #12007, #3792, #9478, #8141, #14632, #7264, #6424 ) ) ;
#3468 = CARTESIAN_POINT ( 'NONE',  ( 10.44112439181167495, 74.26999561062542909, 19.05342973219118363 ) ) ;
#3469 = AXIS2_PLACEMENT_3D ( 'NONE', #7915, #5716, #11646 ) ;
#3470 = DIRECTION ( 'NONE',  ( 0.000000000000000000, 0.000000000000000000, 1.000000000000000000 ) ) ;
#3471 = DIRECTION ( 'NONE',  ( -1.000000000000000000, 0.000000000000000000, 0.000000000000000000 ) ) ;
#3472 = SURFACE_STYLE_FILL_AREA ( #3174 ) ;
#3473 = DIRECTION ( 'NONE',  ( 1.000000000000000000, 0.000000000000000000, 0.000000000000000000 ) ) ;
#3474 = ORIENTED_EDGE ( 'NONE', *, *, #3414, .T. ) ;
#3475 = CARTESIAN_POINT ( 'NONE',  ( 4.024499207728847061, -2.323545700935702119, -3.572172305156873673 ) ) ;
#3476 = ORIENTED_EDGE ( 'NONE', *, *, #14087, .F. ) ;
#3477 = EDGE_CURVE ( 'NONE', #14956, #14203, #10293, .T. ) ;
#3478 = EDGE_CURVE ( 'NONE', #14961, #7570, #11668, .T. ) ;
#3479 = ORIENTED_EDGE ( 'NONE', *, *, #11172, .T. ) ;
#3480 = EDGE_CURVE ( 'NONE', #877, #7720, #3837, .T. ) ;
#3481 = CYLINDRICAL_SURFACE ( 'NONE', #7863, 3.000000000000004441 ) ;
#3482 = DIRECTION ( 'NONE',  ( 0.000000000000000000, 0.000000000000000000, 1.000000000000000000 ) ) ;
#3483 = AXIS2_PLACEMENT_3D ( 'NONE', #5804, #3325, #4686 ) ;
#3484 = ORIENTED_EDGE ( 'NONE', *, *, #11180, .T. ) ;
#3485 = VECTOR ( 'NONE', #5617, 1000.000000000000000 ) ;
#3486 = ORIENTED_EDGE ( 'NONE', *, *, #7477, .T. ) ;
#3487 = DIRECTION ( 'NONE',  ( -0.000000000000000000, 0.000000000000000000, -1.000000000000000000 ) ) ;
#3488 = VERTEX_POINT ( 'NONE', #6098 ) ;
#3489 = ORIENTED_EDGE ( 'NONE', *, *, #744, .T. ) ;
#3490 = CIRCLE ( 'NONE', #7106, 56.99999999999998579 ) ;
#3491 = DIRECTION ( 'NONE',  ( 0.000000000000000000, 0.000000000000000000, 1.000000000000000000 ) ) ;
#3492 = LINE ( 'NONE', #2344, #3695 ) ;
#3493 = CIRCLE ( 'NONE', #14885, 2.649999999999987477 ) ;
#3494 = DIRECTION ( 'NONE',  ( 0.000000000000000000, 0.000000000000000000, 1.000000000000000000 ) ) ;
#3495 = DIRECTION ( 'NONE',  ( 1.000000000000000000, 0.000000000000000000, 0.000000000000000000 ) ) ;
#3496 = EDGE_LOOP ( 'NONE', ( #9002, #4538, #3928, #5576, #3004, #1098, #4357, #305, #4849 ) ) ;
#3497 = CARTESIAN_POINT ( 'NONE',  ( -89.61631465359519666, -37.12029293941281338, -8.000000000000000000 ) ) ;
#3498 = ORIENTED_EDGE ( 'NONE', *, *, #13128, .F. ) ;
#3499 = FACE_OUTER_BOUND ( 'NONE', #7883, .T. ) ;
#3500 = AXIS2_PLACEMENT_3D ( 'NONE', #5033, #244, #9640 ) ;
#3501 = CIRCLE ( 'NONE', #14170, 52.50000000000000711 ) ;
#3502 = AXIS2_PLACEMENT_3D ( 'NONE', #14114, #295, #8554 ) ;
#3503 = CYLINDRICAL_SURFACE ( 'NONE', #948, 60.50000000000000000 ) ;
#3504 = AXIS2_PLACEMENT_3D ( 'NONE', #8822, #3135, #6610 ) ;
#3505 = EDGE_CURVE ( 'NONE', #4977, #10396, #2475, .T. ) ;
#3506 = EDGE_LOOP ( 'NONE', ( #8916, #4758, #949, #1686 ) ) ;
#3507 = DIRECTION ( 'NONE',  ( 0.000000000000000000, 0.000000000000000000, 1.000000000000000000 ) ) ;
#3508 = CARTESIAN_POINT ( 'NONE',  ( 30.18932686484986760, 96.38267619380722806, 13.21651853314491198 ) ) ;
#3509 = ORIENTED_EDGE ( 'NONE', *, *, #8652, .T. ) ;
#3510 = CARTESIAN_POINT ( 'NONE',  ( 89.61631465359491244, 37.12029293941346708, -8.000000000000000000 ) ) ;
#3511 = DIRECTION ( 'NONE',  ( -0.000000000000000000, -0.000000000000000000, -1.000000000000000000 ) ) ;
#3512 = DIRECTION ( 'NONE',  ( 0.000000000000000000, 0.000000000000000000, 1.000000000000000000 ) ) ;
#3513 = CARTESIAN_POINT ( 'NONE',  ( -55.00000000000000000, 0.000000000000000000, -13.00000000000000178 ) ) ;
#3514 = AXIS2_PLACEMENT_3D ( 'NONE', #5749, #9162, #11463 ) ;
#3515 = AXIS2_PLACEMENT_3D ( 'NONE', #2384, #7001, #4602 ) ;
#3516 = CIRCLE ( 'NONE', #9320, 7.500000000000001776 ) ;
#3517 = CARTESIAN_POINT ( 'NONE',  ( -3.999999999999626965, -0.8232339106132875450, -3.430630286862371925 ) ) ;
#3518 = CONTEXT_DEPENDENT_SHAPE_REPRESENTATION ( #12424, #7420 ) ;
#3519 = PLANE ( 'NONE',  #6327 ) ;
#3520 = ORIENTED_EDGE ( 'NONE', *, *, #3332, .F. ) ;
#3521 = DIRECTION ( 'NONE',  ( -0.000000000000000000, -0.000000000000000000, 1.000000000000000000 ) ) ;
#3522 = DIRECTION ( 'NONE',  ( 1.000000000000000000, 1.243449787580175325E-13, 0.000000000000000000 ) ) ;
#3523 = EDGE_CURVE ( 'NONE', #8423, #511, #13635, .T. ) ;
#3524 = AXIS2_PLACEMENT_3D ( 'NONE', #7765, #14326, #2080 ) ;
#3525 = EDGE_CURVE ( 'NONE', #10333, #13430, #3989, .T. ) ;
#3526 = LINE ( 'NONE', #1238, #1051 ) ;
#3527 = AXIS2_PLACEMENT_3D ( 'NONE', #13401, #11203, #12565 ) ;
#3528 = CIRCLE ( 'NONE', #4981, 63.00000000000000000 ) ;
#3529 = CARTESIAN_POINT ( 'NONE',  ( 37.21932736666271779, -89.12622059913267947, -13.00000000000000178 ) ) ;
#3530 = ORIENTED_EDGE ( 'NONE', *, *, #9973, .F. ) ;
#3531 = DIRECTION ( 'NONE',  ( -0.7071067811865479058, 8.659560562354930393E-17, -0.7071067811865472397 ) ) ;
#3532 = VERTEX_POINT ( 'NONE', #1482 ) ;
#3533 = DIRECTION ( 'NONE',  ( 0.000000000000000000, 0.000000000000000000, 1.000000000000000000 ) ) ;
#3534 = CARTESIAN_POINT ( 'NONE',  ( -25.99999999999971223, -45.89934640057541060, -13.00000000000000178 ) ) ;
#3535 = ADVANCED_FACE ( 'NONE', ( #14237 ), #14083, .T. ) ;
#3536 = AXIS2_PLACEMENT_3D ( 'NONE', #5255, #13519, #13234 ) ;
#3537 = CARTESIAN_POINT ( 'NONE',  ( 30.00000000000001066, 97.48846085563154418, -31.00000000000000000 ) ) ;
#3538 = DIRECTION ( 'NONE',  ( -0.000000000000000000, -0.000000000000000000, 1.000000000000000000 ) ) ;
#3539 = AXIS2_PLACEMENT_3D ( 'NONE', #454, #5084, #14349 ) ;
#3540 = VERTEX_POINT ( 'NONE', #4902 ) ;
#3541 = DIRECTION ( 'NONE',  ( 0.000000000000000000, 0.000000000000000000, -1.000000000000000000 ) ) ;
#3542 = CYLINDRICAL_SURFACE ( 'NONE', #3515, 2.649999999999992806 ) ;
#3543 = EDGE_CURVE ( 'NONE', #4701, #4832, #6019, .T. ) ;
#3544 = CARTESIAN_POINT ( 'NONE',  ( 50.00000000000000000, 6.123233995736766085E-15, 13.00000000000000178 ) ) ;
#3545 = CIRCLE ( 'NONE', #12037, 60.50000000000000000 ) ;
#3546 = ORIENTED_EDGE ( 'NONE', *, *, #6983, .T. ) ;
#3547 = AXIS2_PLACEMENT_3D ( 'NONE', #8936, #13571, #12674 ) ;
#3548 = ORIENTED_EDGE ( 'NONE', *, *, #12478, .T. ) ;
#3549 = VERTEX_POINT ( 'NONE', #2616 ) ;
#3550 = DIRECTION ( 'NONE',  ( 1.000000000000000000, 0.000000000000000000, 0.000000000000000000 ) ) ;
#3551 = LINE ( 'NONE', #9523, #14825 ) ;
#3552 = CARTESIAN_POINT ( 'NONE',  ( 3.472371940586087558, 2.614027278893122475, -3.320322319201942207 ) ) ;
#3553 = FACE_OUTER_BOUND ( 'NONE', #6311, .T. ) ;
#3554 = CIRCLE ( 'NONE', #13484, 0.5000000000000038858 ) ;
#3555 = CARTESIAN_POINT ( 'NONE',  ( 0.000000000000000000, 0.000000000000000000, -13.00000000000000178 ) ) ;
#3556 = ORIENTED_EDGE ( 'NONE', *, *, #13066, .F. ) ;
#3557 = ORIENTED_EDGE ( 'NONE', *, *, #11019, .T. ) ;
#3558 = DIRECTION ( 'NONE',  ( 0.000000000000000000, 0.000000000000000000, 1.000000000000000000 ) ) ;
#3559 = CARTESIAN_POINT ( 'NONE',  ( 69.08935777509475429, -68.58935777509547904, 10.49999999999999822 ) ) ;
#3560 = ORIENTED_EDGE ( 'NONE', *, *, #3569, .T. ) ;
#3561 = ORIENTED_EDGE ( 'NONE', *, *, #1434, .T. ) ;
#3562 = PLANE ( 'NONE',  #13211 ) ;
#3563 = CIRCLE ( 'NONE', #11080, 3.000000000000002665 ) ;
#3564 = ORIENTED_EDGE ( 'NONE', *, *, #4887, .F. ) ;
#3565 = ORIENTED_EDGE ( 'NONE', *, *, #9807, .T. ) ;
#3566 = ADVANCED_FACE ( 'NONE', ( #483 ), #9514, .T. ) ;
#3567 = DIRECTION ( 'NONE',  ( 0.000000000000000000, 0.000000000000000000, 1.000000000000000000 ) ) ;
#3568 = CARTESIAN_POINT ( 'NONE',  ( -53.06332297728247482, 7.252293700257352427, -10.50000000000000000 ) ) ;
#3569 = EDGE_CURVE ( 'NONE', #6334, #1115, #12676, .T. ) ;
#3570 = CARTESIAN_POINT ( 'NONE',  ( -49.11971303961688307, -15.88467684210530528, -8.000000000000000000 ) ) ;
#3571 = DIRECTION ( 'NONE',  ( 1.000000000000000000, 0.000000000000000000, 0.000000000000000000 ) ) ;
#3572 = CARTESIAN_POINT ( 'NONE',  ( -10.44112439181167495, 74.26999561062542909, -19.05342973219118008 ) ) ;
#3573 = CARTESIAN_POINT ( 'NONE',  ( -26.99988008862626643, -45.88839665196127271, -10.50000000000000000 ) ) ;
#3574 = ORIENTED_EDGE ( 'NONE', *, *, #12668, .T. ) ;
#3575 = EDGE_CURVE ( 'NONE', #5656, #1886, #3703, .T. ) ;
#3576 = DIRECTION ( 'NONE',  ( 1.000000000000000000, 0.000000000000000000, 0.000000000000000000 ) ) ;
#3577 = CARTESIAN_POINT ( 'NONE',  ( 0.000000000000000000, 0.000000000000000000, 8.000000000000000000 ) ) ;
#3578 = ORIENTED_EDGE ( 'NONE', *, *, #9207, .F. ) ;
#3579 = PRODUCT_DEFINITION ( 'UNKNOWN', '', #4853, #3043 ) ;
#3580 = FILL_AREA_STYLE_COLOUR ( '', #6425 ) ;
#3581 = ORIENTED_EDGE ( 'NONE', *, *, #5772, .F. ) ;
#3582 = CARTESIAN_POINT ( 'NONE',  ( 30.00974697327758989, 96.43868009418279996, 12.76250177908514516 ) ) ;
#3583 = VERTEX_POINT ( 'NONE', #11887 ) ;
#3584 = EDGE_CURVE ( 'NONE', #604, #11699, #8061, .T. ) ;
#3585 = CARTESIAN_POINT ( 'NONE',  ( 40.12029293941316155, -89.61631465359504034, 8.000000000000000000 ) ) ;
#3586 = CARTESIAN_POINT ( 'NONE',  ( 90.11631465359468507, -37.12029293941410657, -10.50000000000000000 ) ) ;
#3587 = CARTESIAN_POINT ( 'NONE',  ( 51.19406879332056093, 13.71740939043382745, -10.50000000000000000 ) ) ;
#3588 = PLANE ( 'NONE',  #11231 ) ;
#3589 = CYLINDRICAL_SURFACE ( 'NONE', #14781, 10.00000000000000178 ) ;
#3590 = DIRECTION ( 'NONE',  ( 1.000000000000000000, 0.000000000000000000, 0.000000000000000000 ) ) ;
#3591 = ORIENTED_EDGE ( 'NONE', *, *, #12772, .F. ) ;
#3592 = DIRECTION ( 'NONE',  ( 0.000000000000000000, -1.287488025362403787E-15, -1.000000000000000000 ) ) ;
#3593 = CARTESIAN_POINT ( 'NONE',  ( -3.679171394226030678, -2.494631558665843407, -0.3503314178412529345 ) ) ;
#3594 = AXIS2_PLACEMENT_3D ( 'NONE', #5170, #4478, #9092 ) ;
#3595 = DIRECTION ( 'NONE',  ( 1.000000000000000000, 0.000000000000000000, 0.000000000000000000 ) ) ;
#3596 = B_SPLINE_CURVE_WITH_KNOTS ( 'NONE', 3,
 ( #12176, #11878, #5264, #12101, #6382, #9646, #1693, #6300, #7380, #13164, #335, #3760, #6233, #8381, #2609, #411, #4972, #9584, #5111, #2759 ),
 .UNSPECIFIED., .F., .F.,
 ( 4, 2, 2, 2, 2, 2, 2, 2, 2, 4 ),
 ( 1.430489624538199204E-17, 0.0009816351435713611961, 0.001472452715357042662, 0.001963270287142724127, 0.002944905430714070578, 0.003926540574285417029, 0.004908175717856764347, 0.005889810861428110798, 0.006871446004999457249, 0.007853081148570804568 ),
 .UNSPECIFIED. ) ;
#3597 = CYLINDRICAL_SURFACE ( 'NONE', #12486, 50.00000000000000000 ) ;
#3598 = ORIENTED_EDGE ( 'NONE', *, *, #2673, .F. ) ;
#3599 =( REPRESENTATION_RELATIONSHIP ('NONE','NONE', #12187, #8006 ) REPRESENTATION_RELATIONSHIP_WITH_TRANSFORMATION ( #11638 )SHAPE_REPRESENTATION_RELATIONSHIP( ) );
#3600 = CARTESIAN_POINT ( 'NONE',  ( -33.48561063518626923, 47.21331623427104063, 10.49999999999999822 ) ) ;
#3601 = ORIENTED_EDGE ( 'NONE', *, *, #374, .F. ) ;
#3602 = DIRECTION ( 'NONE',  ( -0.000000000000000000, -0.000000000000000000, 1.000000000000000000 ) ) ;
#3603 = CARTESIAN_POINT ( 'NONE',  ( 0.000000000000000000, 0.000000000000000000, 3.469446951953614189E-15 ) ) ;
#3604 = EDGE_CURVE ( 'NONE', #4704, #9453, #10817, .T. ) ;
#3605 = EDGE_CURVE ( 'NONE', #8733, #4832, #2003, .T. ) ;
#3606 = CARTESIAN_POINT ( 'NONE',  ( 0.000000000000000000, 0.000000000000000000, -10.50000000000000000 ) ) ;
#3607 = ADVANCED_FACE ( 'NONE', ( #14303 ), #3914, .F. ) ;
#3608 = CARTESIAN_POINT ( 'NONE',  ( -26.00011991137315803, -45.91029614918952007, -10.50000000000000000 ) ) ;
#3609 = ORIENTED_EDGE ( 'NONE', *, *, #12540, .T. ) ;
#3610 = DIRECTION ( 'NONE',  ( 0.000000000000000000, 0.000000000000000000, 1.000000000000000000 ) ) ;
#3611 = VECTOR ( 'NONE', #15029, 1000.000000000000000 ) ;
#3612 = CARTESIAN_POINT ( 'NONE',  ( -3.999999999999996447, -2.309401076758511806, -5.000000000000000888 ) ) ;
#3613 = CARTESIAN_POINT ( 'NONE',  ( -3.999999999999996447, 0.000000000000000000, 0.000000000000000000 ) ) ;
#3614 = ORIENTED_EDGE ( 'NONE', *, *, #880, .T. ) ;
#3615 = EDGE_CURVE ( 'NONE', #5777, #14224, #3462, .T. ) ;
#3616 = ORIENTED_EDGE ( 'NONE', *, *, #979, .T. ) ;
#3617 = ORIENTED_EDGE ( 'NONE', *, *, #3202, .T. ) ;
#3618 = CARTESIAN_POINT ( 'NONE',  ( 11.83867104060235853, 106.3432143034624033, 17.50653253748099303 ) ) ;
#3619 = DIRECTION ( 'NONE',  ( 0.000000000000000000, 0.000000000000000000, -1.000000000000000000 ) ) ;
#3620 = EDGE_CURVE ( 'NONE', #8108, #12802, #5400, .T. ) ;
#3621 = CARTESIAN_POINT ( 'NONE',  ( -36.14014761921588104, 11.74264578624790190, -28.00000000000000000 ) ) ;
#3622 = CARTESIAN_POINT ( 'NONE',  ( 0.000000000000000000, 0.000000000000000000, -10.50000000000000000 ) ) ;
#3623 = DIRECTION ( 'NONE',  ( 0.000000000000000000, 0.000000000000000000, 1.000000000000000000 ) ) ;
#3624 = EDGE_LOOP ( 'NONE', ( #1137, #10558, #14843, #4037 ) ) ;
#3625 = DIRECTION ( 'NONE',  ( 1.000000000000000000, 0.000000000000000000, -0.000000000000000000 ) ) ;
#3626 = VECTOR ( 'NONE', #6753, 1000.000000000000000 ) ;
#3627 = DIRECTION ( 'NONE',  ( 1.000000000000000000, 0.000000000000000000, 0.000000000000000000 ) ) ;
#3628 = CARTESIAN_POINT ( 'NONE',  ( 7.500000000000000000, 62.55197838597913318, 20.00000000000000000 ) ) ;
#3629 = ORIENTED_EDGE ( 'NONE', *, *, #5776, .F. ) ;
#3630 = VERTEX_POINT ( 'NONE', #6240 ) ;
#3631 = FACE_OUTER_BOUND ( 'NONE', #3203, .T. ) ;
#3632 = AXIS2_PLACEMENT_3D ( 'NONE', #13562, #1734, #10995 ) ;
#3633 = VERTEX_POINT ( 'NONE', #14382 ) ;
#3634 = CARTESIAN_POINT ( 'NONE',  ( 9.706953719245472456, 57.06275842387054098, -13.00000000000000178 ) ) ;
#3635 = CIRCLE ( 'NONE', #10900, 0.5000000000000004441 ) ;
#3636 = DIRECTION ( 'NONE',  ( 1.000000000000000000, 0.000000000000000000, 0.000000000000000000 ) ) ;
#3637 = CARTESIAN_POINT ( 'NONE',  ( 99.48933418828643482, -1.674280531759671176, 8.000000000000000000 ) ) ;
#3638 = EDGE_LOOP ( 'NONE', ( #7398, #14292 ) ) ;
#3639 = CARTESIAN_POINT ( 'NONE',  ( -30.00000000000000711, 97.48846085563154418, 26.00000000000000000 ) ) ;
#3640 = DIRECTION ( 'NONE',  ( 0.000000000000000000, 0.000000000000000000, 1.000000000000000000 ) ) ;
#3641 = EDGE_LOOP ( 'NONE', ( #7875, #11828, #3426, #14355, #4996, #3479, #14033 ) ) ;
#3642 = ADVANCED_FACE ( 'NONE', ( #13051 ), #13205, .F. ) ;
#3643 = PRESENTATION_STYLE_ASSIGNMENT (( #9332 ) ) ;
#3644 = CIRCLE ( 'NONE', #7500, 0.5000000000000043299 ) ;
#3645 = CIRCLE ( 'NONE', #1937, 10.00000000000000178 ) ;
#3646 = EDGE_CURVE ( 'NONE', #3918, #14223, #553, .T. ) ;
#3647 = CIRCLE ( 'NONE', #12135, 4.999999999999994671 ) ;
#3648 = CIRCLE ( 'NONE', #12136, 2.649999999999985700 ) ;
#3649 = VERTEX_POINT ( 'NONE', #1409 ) ;
#3650 = CARTESIAN_POINT ( 'NONE',  ( 1.843833675287984673E-15, -4.647091401871394467, -3.572172305156880778 ) ) ;
#3651 = ORIENTED_EDGE ( 'NONE', *, *, #9405, .T. ) ;
#3652 = DIRECTION ( 'NONE',  ( 0.000000000000000000, -0.4999999999999997780, 0.8660254037844388186 ) ) ;
#3653 = LINE ( 'NONE', #2360, #5818 ) ;
#3654 = CIRCLE ( 'NONE', #242, 59.50000000000000000 ) ;
#3655 = FACE_OUTER_BOUND ( 'NONE', #11358, .T. ) ;
#3656 = DIRECTION ( 'NONE',  ( -1.000000000000000000, 0.000000000000000000, -0.000000000000000000 ) ) ;
#3657 = DIRECTION ( 'NONE',  ( -1.000000000000000000, 0.000000000000000000, 0.000000000000000000 ) ) ;
#3658 = AXIS2_PLACEMENT_3D ( 'NONE', #7749, #12396, #13381 ) ;
#3659 = CIRCLE ( 'NONE', #12147, 53.55662432702593634 ) ;
#3660 = ORIENTED_EDGE ( 'NONE', *, *, #7325, .F. ) ;
#3661 = CARTESIAN_POINT ( 'NONE',  ( -51.19406879332065330, -13.71740939043347041, 8.000000000000000000 ) ) ;
#3662 = VERTEX_POINT ( 'NONE', #648 ) ;
#3663 = EDGE_CURVE ( 'NONE', #4909, #2144, #4684, .T. ) ;
#3664 = ADVANCED_FACE ( 'NONE', ( #6619 ), #7762, .T. ) ;
#3665 = EDGE_CURVE ( 'NONE', #10864, #10761, #4204, .T. ) ;
#3666 = CIRCLE ( 'NONE', #268, 0.5000000000000004441 ) ;
#3667 = CARTESIAN_POINT ( 'NONE',  ( -9.115592515563381681, 106.6114291000284027, -19.74294316973679742 ) ) ;
#3668 = DIRECTION ( 'NONE',  ( -0.000000000000000000, -0.000000000000000000, -1.000000000000000000 ) ) ;
#3669 = CIRCLE ( 'NONE', #8014, 56.99999999999999289 ) ;
#3670 = DIRECTION ( 'NONE',  ( -0.000000000000000000, -0.000000000000000000, -1.000000000000000000 ) ) ;
#3671 = EDGE_CURVE ( 'NONE', #9386, #5754, #11725, .T. ) ;
#3672 = LINE ( 'NONE', #11952, #14160 ) ;
#3673 = AXIS2_PLACEMENT_3D ( 'NONE', #5382, #10147, #1810 ) ;
#3674 = EDGE_LOOP ( 'NONE', ( #6882, #7316, #13379, #9845, #10345 ) ) ;
#3675 = DIRECTION ( 'NONE',  ( 0.000000000000000000, 0.000000000000000000, 1.000000000000000000 ) ) ;
#3676 = ORIENTED_EDGE ( 'NONE', *, *, #10787, .F. ) ;
#3677 = EDGE_LOOP ( 'NONE', ( #13640, #4257, #11348, #3140 ) ) ;
#3678 = LINE ( 'NONE', #4588, #7751 ) ;
#3679 = CYLINDRICAL_SURFACE ( 'NONE', #4188, 3.000000000000002665 ) ;
#3680 = AXIS2_PLACEMENT_3D ( 'NONE', #9648, #478, #7524 ) ;
#3681 = FACE_OUTER_BOUND ( 'NONE', #4322, .T. ) ;
#3682 = DIRECTION ( 'NONE',  ( -1.000000000000000000, 0.000000000000000000, 0.000000000000000000 ) ) ;
#3683 = ORIENTED_EDGE ( 'NONE', *, *, #5722, .F. ) ;
#3684 = AXIS2_PLACEMENT_3D ( 'NONE', #4366, #8982, #5503 ) ;
#3685 = ORIENTED_EDGE ( 'NONE', *, *, #1113, .T. ) ;
#3686 = CARTESIAN_POINT ( 'NONE',  ( 0.000000000000000000, 0.000000000000000000, -8.000000000000000000 ) ) ;
#3687 = CARTESIAN_POINT ( 'NONE',  ( 45.89934640057532533, -26.49999999999987566, 10.49999999999999822 ) ) ;
#3688 = DIRECTION ( 'NONE',  ( 0.000000000000000000, 0.000000000000000000, -1.000000000000000000 ) ) ;
#3689 = ORIENTED_EDGE ( 'NONE', *, *, #7960, .T. ) ;
#3690 = CIRCLE ( 'NONE', #12175, 3.000000000000002665 ) ;
#3691 = EDGE_CURVE ( 'NONE', #5730, #4479, #10252, .T. ) ;
#3692 = VERTEX_POINT ( 'NONE', #1919 ) ;
#3693 = ORIENTED_EDGE ( 'NONE', *, *, #10596, .F. ) ;
#3694 = ADVANCED_FACE ( 'NONE', ( #12407 ), #9071, .F. ) ;
#3695 = VECTOR ( 'NONE', #6961, 999.9999999999998863 ) ;
#3696 = CARTESIAN_POINT ( 'NONE',  ( 10.80358476664835266, 106.4534462909512769, 18.76728514983858531 ) ) ;
#3697 = CARTESIAN_POINT ( 'NONE',  ( 5.204748896376250896E-15, 85.00000000000000000, 31.00000000000000000 ) ) ;
#3698 = CARTESIAN_POINT ( 'NONE',  ( 0.000000000000000000, 0.000000000000000000, 0.000000000000000000 ) ) ;
#3699 = SURFACE_STYLE_FILL_AREA ( #10666 ) ;
#3700 = CARTESIAN_POINT ( 'NONE',  ( 12.50000000000000000, 61.74746958378133144, -15.00000000000000355 ) ) ;
#3701 = ORIENTED_EDGE ( 'NONE', *, *, #14984, .F. ) ;
#3702 = ORIENTED_EDGE ( 'NONE', *, *, #81, .T. ) ;
#3703 = CIRCLE ( 'NONE', #14619, 3.000000000000002665 ) ;
#3704 = ORIENTED_EDGE ( 'NONE', *, *, #9865, .F. ) ;
#3705 = ORIENTED_EDGE ( 'NONE', *, *, #1912, .T. ) ;
#3706 = CARTESIAN_POINT ( 'NONE',  ( -26.00011991137315803, -45.91029614918952007, -13.00000000000000178 ) ) ;
#3707 = CARTESIAN_POINT ( 'NONE',  ( 37.62029293941316155, -89.61631465359504034, -13.00000000000000178 ) ) ;
#3708 = DIRECTION ( 'NONE',  ( 0.000000000000000000, 0.000000000000000000, -1.000000000000000000 ) ) ;
#3709 = ORIENTED_EDGE ( 'NONE', *, *, #610, .F. ) ;
#3710 = EDGE_CURVE ( 'NONE', #11690, #10452, #3715, .T. ) ;
#3711 = EDGE_CURVE ( 'NONE', #1924, #12179, #12267, .T. ) ;
#3712 = ORIENTED_EDGE ( 'NONE', *, *, #2547, .T. ) ;
#3713 = DIRECTION ( 'NONE',  ( 1.000000000000000000, 0.000000000000000000, 0.000000000000000000 ) ) ;
#3714 = ORIENTED_EDGE ( 'NONE', *, *, #5374, .F. ) ;
#3715 = CIRCLE ( 'NONE', #11716, 63.00000000000000000 ) ;
#3716 = CARTESIAN_POINT ( 'NONE',  ( 56.43380494353997534, 12.86891638962136319, -13.00000000000000178 ) ) ;
#3717 = DIRECTION ( 'NONE',  ( 0.000000000000000000, 0.000000000000000000, 1.000000000000000000 ) ) ;
#3718 = AXIS2_PLACEMENT_3D ( 'NONE', #13294, #10941, #7290 ) ;
#3719 = CARTESIAN_POINT ( 'NONE',  ( -68.01302780753309207, 65.64523757230344359, -8.000000000000000000 ) ) ;
#3720 = DIRECTION ( 'NONE',  ( 0.000000000000000000, 0.000000000000000000, 1.000000000000000000 ) ) ;
#3721 = EDGE_CURVE ( 'NONE', #5754, #900, #1855, .T. ) ;
#3722 = AXIS2_PLACEMENT_3D ( 'NONE', #15014, #7091, #1191 ) ;
#3723 = CARTESIAN_POINT ( 'NONE',  ( -7.787661217455939422, 74.59514674284385194, -20.00000000000000000 ) ) ;
#3724 = CARTESIAN_POINT ( 'NONE',  ( 89.61631465359468507, -37.12029293941410657, -10.50000000000000000 ) ) ;
#3725 = ORIENTED_EDGE ( 'NONE', *, *, #1890, .F. ) ;
#3726 = B_SPLINE_CURVE_WITH_KNOTS ( 'NONE', 3,
 ( #5932, #10571, #4802, #7140, #2519, #9415, #13007, #14064 ),
 .UNSPECIFIED., .F., .F.,
 ( 4, 2, 2, 4 ),
 ( 2.465131517060789857E-07, 0.001183067374689849563, 0.001774477805458922215, 0.002365888236227995083 ),
 .UNSPECIFIED. ) ;
#3727 = FACE_OUTER_BOUND ( 'NONE', #11669, .T. ) ;
#3728 = AXIS2_PLACEMENT_3D ( 'NONE', #13448, #7669, #12314 ) ;
#3729 = ORIENTED_EDGE ( 'NONE', *, *, #8166, .F. ) ;
#3730 = ORIENTED_EDGE ( 'NONE', *, *, #13168, .F. ) ;
#3731 = ORIENTED_EDGE ( 'NONE', *, *, #14454, .T. ) ;
#3732 = AXIS2_PLACEMENT_3D ( 'NONE', #10431, #106, #13788 ) ;
#3733 = CARTESIAN_POINT ( 'NONE',  ( 12.39897948556635576, 94.18739463280904545, 16.00000000000000000 ) ) ;
#3734 = ORIENTED_EDGE ( 'NONE', *, *, #10885, .T. ) ;
#3735 = LINE ( 'NONE', #388, #14811 ) ;
#3736 = PLANE ( 'NONE',  #9333 ) ;
#3737 = CARTESIAN_POINT ( 'NONE',  ( 57.06275842387049835, -9.706953719245678514, -13.00000000000000178 ) ) ;
#3738 = LINE ( 'NONE', #8359, #7494 ) ;
#3739 = DIRECTION ( 'NONE',  ( -0.000000000000000000, -0.000000000000000000, -1.000000000000000000 ) ) ;
#3740 = ORIENTED_EDGE ( 'NONE', *, *, #408, .T. ) ;
#3741 = AXIS2_PLACEMENT_3D ( 'NONE', #9280, #9051, #5860 ) ;
#3742 = CARTESIAN_POINT ( 'NONE',  ( 92.61631465359468507, -37.12029293941410657, 8.000000000000000000 ) ) ;
#3743 = VECTOR ( 'NONE', #1369, 1000.000000000000000 ) ;
#3744 = ORIENTED_EDGE ( 'NONE', *, *, #10613, .F. ) ;
#3745 = DIRECTION ( 'NONE',  ( -0.000000000000000000, -0.000000000000000000, -1.000000000000000000 ) ) ;
#3746 = DIRECTION ( 'NONE',  ( -1.000000000000000000, 0.000000000000000000, 0.000000000000000000 ) ) ;
#3747 = CARTESIAN_POINT ( 'NONE',  ( 3.999999999999996447, 2.309401076758498039, -3.433295621305378020 ) ) ;
#3748 = LINE ( 'NONE', #7370, #9772 ) ;
#3749 = ORIENTED_EDGE ( 'NONE', *, *, #12954, .T. ) ;
#3750 = ORIENTED_EDGE ( 'NONE', *, *, #13962, .F. ) ;
#3751 = CIRCLE ( 'NONE', #7373, 56.99999999999999289 ) ;
#3752 = EDGE_CURVE ( 'NONE', #13429, #14961, #3219, .T. ) ;
#3753 = CARTESIAN_POINT ( 'NONE',  ( 6.917888187663118416, 52.54657765281190507, -13.00000000000000178 ) ) ;
#3754 = AXIS2_PLACEMENT_3D ( 'NONE', #8858, #6338, #905 ) ;
#3755 = ORIENTED_EDGE ( 'NONE', *, *, #7926, .T. ) ;
#3756 = DIRECTION ( 'NONE',  ( -0.000000000000000000, -0.000000000000000000, 1.000000000000000000 ) ) ;
#3757 = EDGE_CURVE ( 'NONE', #9770, #8423, #7573, .T. ) ;
#3758 = CARTESIAN_POINT ( 'NONE',  ( -99.48933418828642061, 1.674280531760366397, -8.000000000000000000 ) ) ;
#3759 = EDGE_CURVE ( 'NONE', #9923, #2530, #13174, .T. ) ;
#3760 = CARTESIAN_POINT ( 'NONE',  ( -32.65306121041741250, 101.8676703390407141, -14.32076206672372543 ) ) ;
#3761 = CARTESIAN_POINT ( 'NONE',  ( -42.89934640057513349, 26.50000000000019540, -13.00000000000000178 ) ) ;
#3762 = AXIS2_PLACEMENT_3D ( 'NONE', #512, #588, #10989 ) ;
#3763 = ORIENTED_EDGE ( 'NONE', *, *, #4719, .T. ) ;
#3764 = CIRCLE ( 'NONE', #12006, 3.000000000000002665 ) ;
#3765 = ORIENTED_EDGE ( 'NONE', *, *, #665, .T. ) ;
#3766 = DIRECTION ( 'NONE',  ( -1.000000000000000000, 0.000000000000000000, 0.000000000000000000 ) ) ;
#3767 = FACE_OUTER_BOUND ( 'NONE', #5152, .T. ) ;
#3768 = AXIS2_PLACEMENT_3D ( 'NONE', #6376, #191, #4121 ) ;
#3769 = DIRECTION ( 'NONE',  ( -0.000000000000000000, -0.000000000000000000, 1.000000000000000000 ) ) ;
#3770 = VERTEX_POINT ( 'NONE', #5272 ) ;
#3771 = EDGE_CURVE ( 'NONE', #14203, #12897, #10964, .T. ) ;
#3772 = AXIS2_PLACEMENT_3D ( 'NONE', #12929, #5935, #6003 ) ;
#3773 = ORIENTED_EDGE ( 'NONE', *, *, #853, .T. ) ;
#3774 = CARTESIAN_POINT ( 'NONE',  ( 0.000000000000000000, 0.000000000000000000, 13.00000000000000178 ) ) ;
#3775 = ADVANCED_FACE ( 'NONE', ( #12184 ), #9887, .F. ) ;
#3776 = CARTESIAN_POINT ( 'NONE',  ( 7.829984960685308693, 106.7136390683880336, 20.00000000000000355 ) ) ;
#3777 = VECTOR ( 'NONE', #12681, 1000.000000000000000 ) ;
#3778 = CARTESIAN_POINT ( 'NONE',  ( -47.21331623427138879, -33.48561063518577896, -13.00000000000000178 ) ) ;
#3779 = FACE_BOUND ( 'NONE', #8908, .T. ) ;
#3780 = SHAPE_REPRESENTATION_RELATIONSHIP ( 'NONE' , 'NONE' ,  #12767, #1675 ) ;
#3781 = DIRECTION ( 'NONE',  ( -0.000000000000000000, -0.000000000000000000, 1.000000000000000000 ) ) ;
#3782 = ORIENTED_EDGE ( 'NONE', *, *, #13127, .F. ) ;
#3783 = ORIENTED_EDGE ( 'NONE', *, *, #9761, .F. ) ;
#3784 = APPLICATION_CONTEXT ( 'automotive_design' ) ;
#3785 = ORIENTED_EDGE ( 'NONE', *, *, #2124, .F. ) ;
#3786 = CIRCLE ( 'NONE', #12516, 100.0000000000000000 ) ;
#3787 = CARTESIAN_POINT ( 'NONE',  ( -14.00000000000000000, 0.000000000000000000, -45.50000000000000000 ) ) ;
#3788 = DIRECTION ( 'NONE',  ( 0.000000000000000000, 0.000000000000000000, 1.000000000000000000 ) ) ;
#3789 = AXIS2_PLACEMENT_3D ( 'NONE', #13358, #13217, #6500 ) ;
#3790 = CARTESIAN_POINT ( 'NONE',  ( -97.41488903138106537, 0.2790467552942557661, -13.00000000000000178 ) ) ;
#3791 = EDGE_LOOP ( 'NONE', ( #11149, #5966, #14013, #14976 ) ) ;
#3792 = ORIENTED_EDGE ( 'NONE', *, *, #12667, .T. ) ;
#3793 = CARTESIAN_POINT ( 'NONE',  ( 12.86891638962116247, -56.43380494354001087, 8.000000000000000000 ) ) ;
#3794 = ORIENTED_EDGE ( 'NONE', *, *, #3605, .T. ) ;
#3795 = AXIS2_PLACEMENT_3D ( 'NONE', #1478, #6016, #6096 ) ;
#3796 = DIRECTION ( 'NONE',  ( -0.2941176470588241498, 0.9557692240748186796, 0.000000000000000000 ) ) ;
#3797 = CARTESIAN_POINT ( 'NONE',  ( 0.6640947660592916302, -4.471078309994156896, -3.602146406945703649 ) ) ;
#3798 = DIRECTION ( 'NONE',  ( -0.000000000000000000, -0.000000000000000000, 1.000000000000000000 ) ) ;
#3799 = EDGE_CURVE ( 'NONE', #2645, #5275, #12448, .T. ) ;
#3800 = CYLINDRICAL_SURFACE ( 'NONE', #14826, 56.99999999999999289 ) ;
#3801 = DIRECTION ( 'NONE',  ( 0.000000000000000000, 0.000000000000000000, -1.000000000000000000 ) ) ;
#3802 = ADVANCED_FACE ( 'NONE', ( #12488 ), #1171, .T. ) ;
#3803 = VERTEX_POINT ( 'NONE', #6922 ) ;
#3804 = DIRECTION ( 'NONE',  ( -1.000000000000000000, -1.065814103640150279E-14, 0.000000000000000000 ) ) ;
#3805 = AXIS2_PLACEMENT_3D ( 'NONE', #2842, #7759, #6387 ) ;
#3806 = EDGE_LOOP ( 'NONE', ( #9086, #7248 ) ) ;
#3807 = EDGE_LOOP ( 'NONE', ( #4917, #12571, #7703, #10159 ) ) ;
#3808 = CARTESIAN_POINT ( 'NONE',  ( 3.999999999999996447, -0.3979232138631224602, 2.803679055411734122E-15 ) ) ;
#3809 = ADVANCED_FACE ( 'NONE', ( #6846 ), #6987, .T. ) ;
#3810 = DIRECTION ( 'NONE',  ( 1.000000000000000000, 0.000000000000000000, 0.000000000000000000 ) ) ;
#3811 = AXIS2_PLACEMENT_3D ( 'NONE', #14726, #2107, #13649 ) ;
#3812 = CARTESIAN_POINT ( 'NONE',  ( -3.492805317593278058, 46.55633131742322917, -10.50000000000000000 ) ) ;
#3813 = CARTESIAN_POINT ( 'NONE',  ( -7.500000000000000888, 62.55197838597913318, -20.00000000000000000 ) ) ;
#3814 = CARTESIAN_POINT ( 'NONE',  ( -42.04772703543551415, -32.26435573746212526, -13.00000000000000178 ) ) ;
#3815 = DIRECTION ( 'NONE',  ( 0.000000000000000000, 0.000000000000000000, 1.000000000000000000 ) ) ;
#3816 = CIRCLE ( 'NONE', #12299, 0.5000000000000073275 ) ;
#3817 = DIRECTION ( 'NONE',  ( 0.000000000000000000, -1.000000000000000000, -0.000000000000000000 ) ) ;
#3818 = EDGE_CURVE ( 'NONE', #5159, #13568, #12686, .T. ) ;
#3819 = VERTEX_POINT ( 'NONE', #10193 ) ;
#3820 = DIRECTION ( 'NONE',  ( 0.000000000000000000, 0.000000000000000000, 1.000000000000000000 ) ) ;
#3821 = ORIENTED_EDGE ( 'NONE', *, *, #8150, .F. ) ;
#3822 = DIRECTION ( 'NONE',  ( 0.000000000000000000, 0.000000000000000000, -1.000000000000000000 ) ) ;
#3823 = CARTESIAN_POINT ( 'NONE',  ( 72.70695371924547601, 57.06275842387054098, -13.00000000000000178 ) ) ;
#3824 = CARTESIAN_POINT ( 'NONE',  ( 89.61631465359468507, -37.12029293941410657, 10.49999999999999822 ) ) ;
#3825 = CARTESIAN_POINT ( 'NONE',  ( -30.80502811811232888, -49.00442420935981147, -10.50000000000000000 ) ) ;
#3826 = VERTEX_POINT ( 'NONE', #11506 ) ;
#3827 = DIRECTION ( 'NONE',  ( 0.000000000000000000, 0.000000000000000000, -1.000000000000000000 ) ) ;
#3828 = ORIENTED_EDGE ( 'NONE', *, *, #4231, .F. ) ;
#3829 = CARTESIAN_POINT ( 'NONE',  ( 0.000000000000000000, 0.000000000000000000, 0.000000000000000000 ) ) ;
#3830 = CARTESIAN_POINT ( 'NONE',  ( -45.91029614918924295, 26.00011991137363765, 10.49999999999999822 ) ) ;
#3831 = DIRECTION ( 'NONE',  ( -0.000000000000000000, -0.000000000000000000, -1.000000000000000000 ) ) ;
#3832 = DIRECTION ( 'NONE',  ( 1.000000000000000000, 0.000000000000000000, 0.000000000000000000 ) ) ;
#3833 = AXIS2_PLACEMENT_3D ( 'NONE', #6803, #7947, #4108 ) ;
#3834 = ORIENTED_EDGE ( 'NONE', *, *, #8234, .F. ) ;
#3835 = PLANE ( 'NONE',  #10577 ) ;
#3836 = DIRECTION ( 'NONE',  ( 0.000000000000000000, 0.000000000000000000, 1.000000000000000000 ) ) ;
#3837 = LINE ( 'NONE', #2696, #10966 ) ;
#3838 = EDGE_CURVE ( 'NONE', #6551, #9479, #5643, .T. ) ;
#3839 = EDGE_CURVE ( 'NONE', #4879, #3532, #10980, .T. ) ;
#3840 = EDGE_LOOP ( 'NONE', ( #7818, #5429, #4501, #10790 ) ) ;
#3841 = CYLINDRICAL_SURFACE ( 'NONE', #7284, 63.00000000000000000 ) ;
#3842 = VERTEX_POINT ( 'NONE', #3448 ) ;
#3843 = DIRECTION ( 'NONE',  ( 0.000000000000000000, 0.000000000000000000, -1.000000000000000000 ) ) ;
#3844 = ORIENTED_EDGE ( 'NONE', *, *, #275, .T. ) ;
#3845 = DIRECTION ( 'NONE',  ( 1.000000000000000000, 0.000000000000000000, 0.000000000000000000 ) ) ;
#3846 = DIRECTION ( 'NONE',  ( -0.000000000000000000, -0.000000000000000000, 1.000000000000000000 ) ) ;
#3847 = SURFACE_STYLE_FILL_AREA ( #9447 ) ;
#3848 = PLANE ( 'NONE',  #13722 ) ;
#3849 = ORIENTED_EDGE ( 'NONE', *, *, #10637, .F. ) ;
#3850 = PRODUCT_DEFINITION ( 'UNKNOWN', '', #729, #11088 ) ;
#3851 = DIRECTION ( 'NONE',  ( 0.000000000000000000, 0.000000000000000000, 1.000000000000000000 ) ) ;
#3852 = CARTESIAN_POINT ( 'NONE',  ( 56.43380494353997534, 12.86891638962136319, -10.50000000000000000 ) ) ;
#3853 = DIRECTION ( 'NONE',  ( -0.000000000000000000, 0.000000000000000000, -1.000000000000000000 ) ) ;
#3854 = EDGE_CURVE ( 'NONE', #12353, #6653, #6601, .T. ) ;
#3856 = EDGE_LOOP ( 'NONE', ( #6831, #9459, #13273, #1873, #12208, #4144, #13395 ) ) ;
#3855 = ADVANCED_FACE ( 'NONE', ( #11346 ), #14990, .F. ) ;
#3857 = ORIENTED_EDGE ( 'NONE', *, *, #2547, .F. ) ;
#3858 = DIRECTION ( 'NONE',  ( 1.000000000000000000, 0.000000000000000000, -0.000000000000000000 ) ) ;
#3859 = ORIENTED_EDGE ( 'NONE', *, *, #5983, .F. ) ;
#3860 = ADVANCED_FACE ( 'NONE', ( #13931 ), #4659, .T. ) ;
#3861 = DIRECTION ( 'NONE',  ( 0.000000000000000000, 0.000000000000000000, 1.000000000000000000 ) ) ;
#3862 = CARTESIAN_POINT ( 'NONE',  ( -0.2790467552932288098, -97.41488903138106537, -10.50000000000000000 ) ) ;
#3863 = FACE_OUTER_BOUND ( 'NONE', #3094, .T. ) ;
#3864 = AXIS2_PLACEMENT_3D ( 'NONE', #10114, #14756, #4354 ) ;
#3865 = ORIENTED_EDGE ( 'NONE', *, *, #1431, .T. ) ;
#3866 = DIRECTION ( 'NONE',  ( 1.000000000000000000, 0.000000000000000000, 0.000000000000000000 ) ) ;
#3867 = FACE_OUTER_BOUND ( 'NONE', #14651, .T. ) ;
#3868 = ORIENTED_EDGE ( 'NONE', *, *, #302, .F. ) ;
#3869 = FACE_OUTER_BOUND ( 'NONE', #13705, .T. ) ;
#3870 = ORIENTED_EDGE ( 'NONE', *, *, #5046, .T. ) ;
#3871 =( GEOMETRIC_REPRESENTATION_CONTEXT ( 3 ) GLOBAL_UNCERTAINTY_ASSIGNED_CONTEXT ( ( #13249 ) ) GLOBAL_UNIT_ASSIGNED_CONTEXT ( ( #908, #6949, #971 ) ) REPRESENTATION_CONTEXT ( 'NONE', 'WORKASPACE' ) );
#3872 = ORIENTED_EDGE ( 'NONE', *, *, #3993, .F. ) ;
#3873 = CARTESIAN_POINT ( 'NONE',  ( -33.48561063518626923, 47.21331623427104063, -13.00000000000000178 ) ) ;
#3874 = AXIS2_PLACEMENT_3D ( 'NONE', #12070, #11924, #5155 ) ;
#3875 = DIRECTION ( 'NONE',  ( -0.000000000000000000, -0.000000000000000000, -1.000000000000000000 ) ) ;
#3876 = ADVANCED_FACE ( 'NONE', ( #12706 ), #12558, .T. ) ;
#3877 = ORIENTED_EDGE ( 'NONE', *, *, #10834, .F. ) ;
#3878 = DIRECTION ( 'NONE',  ( -1.000000000000000000, 0.000000000000000000, 0.000000000000000000 ) ) ;
#3879 = EDGE_CURVE ( 'NONE', #7182, #1468, #8792, .T. ) ;
#3880 = LINE ( 'NONE', #14275, #11766 ) ;
#3881 = DIRECTION ( 'NONE',  ( 0.000000000000000000, 0.000000000000000000, 1.000000000000000000 ) ) ;
#3882 = CARTESIAN_POINT ( 'NONE',  ( -45.89934640057513349, 26.50000000000019540, -13.00000000000000178 ) ) ;
#3883 = PRODUCT_DEFINITION_FORMATION_WITH_SPECIFIED_SOURCE ( 'ANY', '', #12162, .NOT_KNOWN. ) ;
#3884 = CIRCLE ( 'NONE', #9678, 100.0000000000000000 ) ;
#3885 = DIRECTION ( 'NONE',  ( 0.000000000000000000, 0.000000000000000000, -1.000000000000000000 ) ) ;
#3886 = ORIENTED_EDGE ( 'NONE', *, *, #11325, .F. ) ;
#3887 = EDGE_CURVE ( 'NONE', #14486, #2928, #3526, .T. ) ;
#3888 = AXIS2_PLACEMENT_3D ( 'NONE', #2899, #1624, #11807 ) ;
#3889 =( NAMED_UNIT ( * ) PLANE_ANGLE_UNIT ( ) SI_UNIT ( $, .RADIAN. ) );
#3890 = VERTEX_POINT ( 'NONE', #9354 ) ;
#3891 = AXIS2_PLACEMENT_3D ( 'NONE', #5993, #536, #8432 ) ;
#3892 = CARTESIAN_POINT ( 'NONE',  ( -12.37198577373457553, 106.2823362334109447, -16.13593661559556836 ) ) ;
#3893 = CYLINDRICAL_SURFACE ( 'NONE', #2018, 5.000000000000001776 ) ;
#3894 = FACE_OUTER_BOUND ( 'NONE', #14344, .T. ) ;
#3895 = EDGE_CURVE ( 'NONE', #13630, #14464, #1531, .T. ) ;
#3896 = AXIS2_PLACEMENT_3D ( 'NONE', #4947, #11938, #8494 ) ;
#3897 = DIRECTION ( 'NONE',  ( -0.000000000000000000, -0.000000000000000000, -1.000000000000000000 ) ) ;
#3898 = ADVANCED_FACE ( 'NONE', ( #3298 ), #6760, .T. ) ;
#3899 = ORIENTED_EDGE ( 'NONE', *, *, #4764, .T. ) ;
#3900 = DIRECTION ( 'NONE',  ( -1.000000000000000000, 0.000000000000000000, 0.000000000000000000 ) ) ;
#3901 = AXIS2_PLACEMENT_3D ( 'NONE', #13800, #12513, #11374 ) ;
#3902 = ORIENTED_EDGE ( 'NONE', *, *, #131, .F. ) ;
#3903 = AXIS2_PLACEMENT_3D ( 'NONE', #14115, #3798, #12902 ) ;
#3904 = DIRECTION ( 'NONE',  ( 1.000000000000000000, 0.000000000000000000, 0.000000000000000000 ) ) ;
#3905 = DIRECTION ( 'NONE',  ( -1.000000000000000000, 0.000000000000000000, 0.000000000000000000 ) ) ;
#3906 = LINE ( 'NONE', #1626, #13572 ) ;
#3907 = DIRECTION ( 'NONE',  ( -1.000000000000000000, 0.000000000000000000, 0.000000000000000000 ) ) ;
#3908 = CARTESIAN_POINT ( 'NONE',  ( -7.500000000000000888, 94.70348462437907244, 20.00000000000000000 ) ) ;
#3909 = AXIS2_PLACEMENT_3D ( 'NONE', #5757, #8258, #5826 ) ;
#3910 = ORIENTED_EDGE ( 'NONE', *, *, #2026, .F. ) ;
#3911 = DIRECTION ( 'NONE',  ( -0.5000000000000051070, 1.060575238724903217E-16, -0.8660254037844355990 ) ) ;
#3912 = CIRCLE ( 'NONE', #1489, 0.5000000000000004441 ) ;
#3913 = CYLINDRICAL_SURFACE ( 'NONE', #7642, 60.50000000000000000 ) ;
#3914 = CYLINDRICAL_SURFACE ( 'NONE', #10489, 0.5000000000000022204 ) ;
#3915 = PRODUCT_DEFINITION_SHAPE ( 'NONE', 'NONE',  #15041 ) ;
#3916 = ORIENTED_EDGE ( 'NONE', *, *, #6890, .T. ) ;
#3917 = DIRECTION ( 'NONE',  ( 0.5000000000000013323, -0.8660254037844379305, 0.000000000000000000 ) ) ;
#3918 = VERTEX_POINT ( 'NONE', #5640 ) ;
#3919 = AXIS2_PLACEMENT_3D ( 'NONE', #7800, #2871, #1811 ) ;
#3920 = CARTESIAN_POINT ( 'NONE',  ( -34.12029293941441210, -89.61631465359452875, -8.000000000000000000 ) ) ;
#3921 = ORIENTED_EDGE ( 'NONE', *, *, #532, .T. ) ;
#3922 = AXIS2_PLACEMENT_3D ( 'NONE', #2838, #8524, #7450 ) ;
#3923 = CARTESIAN_POINT ( 'NONE',  ( 10.19763225997207634, 62.16969414240131897, -19.21937000502254023 ) ) ;
#3924 = CIRCLE ( 'NONE', #12894, 10.00000000000000355 ) ;
#3925 = LINE ( 'NONE', #1567, #6597 ) ;
#3926 = DIRECTION ( 'NONE',  ( 0.000000000000000000, 0.000000000000000000, 1.000000000000000000 ) ) ;
#3927 = FACE_OUTER_BOUND ( 'NONE', #11718, .T. ) ;
#3928 = ORIENTED_EDGE ( 'NONE', *, *, #2548, .T. ) ;
#3929 = EDGE_LOOP ( 'NONE', ( #14003, #12873, #4799, #14019 ) ) ;
#3930 = CYLINDRICAL_SURFACE ( 'NONE', #12734, 3.000000000000002665 ) ;
#3931 = DIRECTION ( 'NONE',  ( 1.000000000000000000, 0.000000000000000000, 0.000000000000000000 ) ) ;
#3932 = AXIS2_PLACEMENT_3D ( 'NONE', #3138, #5420, #10269 ) ;
#3933 = DIRECTION ( 'NONE',  ( -1.000000000000000000, 0.000000000000000000, 0.000000000000000000 ) ) ;
#3934 = ORIENTED_EDGE ( 'NONE', *, *, #5280, .T. ) ;
#3935 = ORIENTED_EDGE ( 'NONE', *, *, #14014, .T. ) ;
#3936 = CYLINDRICAL_SURFACE ( 'NONE', #14676, 59.50000000000000000 ) ;
#3937 = ORIENTED_EDGE ( 'NONE', *, *, #2437, .T. ) ;
#3938 = CYLINDRICAL_SURFACE ( 'NONE', #7277, 60.50000000000000000 ) ;
#3939 = EDGE_CURVE ( 'NONE', #10230, #9910, #5523, .T. ) ;
#3940 = ADVANCED_FACE ( 'NONE', ( #3894 ), #466, .F. ) ;
#3941 = DIRECTION ( 'NONE',  ( -1.000000000000000000, 0.000000000000000000, 0.000000000000000000 ) ) ;
#3942 = SURFACE_STYLE_USAGE ( .BOTH. , #14334 ) ;
#3943 = EDGE_CURVE ( 'NONE', #3062, #1186, #11722, .T. ) ;
#3944 = EDGE_CURVE ( 'NONE', #5657, #4604, #13409, .T. ) ;
#3945 = DIRECTION ( 'NONE',  ( 0.000000000000000000, 0.000000000000000000, 1.000000000000000000 ) ) ;
#3946 = CARTESIAN_POINT ( 'NONE',  ( -52.54657765281192638, 6.917888187662934563, -8.000000000000000000 ) ) ;
#3947 = CIRCLE ( 'NONE', #12671, 100.0000000000000000 ) ;
#3948 = ORIENTED_EDGE ( 'NONE', *, *, #2165, .F. ) ;
#3949 = DIRECTION ( 'NONE',  ( 0.000000000000000000, 0.000000000000000000, 1.000000000000000000 ) ) ;
#3950 = ORIENTED_EDGE ( 'NONE', *, *, #13497, .T. ) ;
#3951 = AXIS2_PLACEMENT_3D ( 'NONE', #10216, #14017, #1122 ) ;
#3952 = ORIENTED_EDGE ( 'NONE', *, *, #14952, .F. ) ;
#3953 = CARTESIAN_POINT ( 'NONE',  ( -34.62083247296263266, -87.95718916809180143, 8.000000000000000000 ) ) ;
#3954 = CARTESIAN_POINT ( 'NONE',  ( 31.50188001269984994, 102.2577498558884486, -11.65822132526735899 ) ) ;
#3955 = CIRCLE ( 'NONE', #5879, 2.649999999999985700 ) ;
#3956 = CARTESIAN_POINT ( 'NONE',  ( 5.204748896376250896E-15, 85.00000000000000000, 46.00000000000000000 ) ) ;
#3957 = DIRECTION ( 'NONE',  ( 1.000000000000000000, 0.000000000000000000, 0.000000000000000000 ) ) ;
#3958 = DIRECTION ( 'NONE',  ( -0.5000000000000009992, 0.000000000000000000, 0.8660254037844380415 ) ) ;
#3959 = DIRECTION ( 'NONE',  ( -1.000000000000000000, 0.000000000000000000, 0.000000000000000000 ) ) ;
#3960 = ITEM_DEFINED_TRANSFORMATION ( 'NONE', 'NONE', #5313,  #5108 ) ;
#3961 = ORIENTED_EDGE ( 'NONE', *, *, #593, .T. ) ;
#3962 = DIRECTION ( 'NONE',  ( 1.000000000000000000, 0.000000000000000000, 0.000000000000000000 ) ) ;
#3963 = VECTOR ( 'NONE', #9131, 1000.000000000000000 ) ;
#3964 = ORIENTED_EDGE ( 'NONE', *, *, #13412, .T. ) ;
#3965 = EDGE_CURVE ( 'NONE', #1743, #2090, #7825, .T. ) ;
#3966 = CARTESIAN_POINT ( 'NONE',  ( -48.29629131445344115, -12.94095225512594816, 8.000000000000000000 ) ) ;
#3967 = FACE_OUTER_BOUND ( 'NONE', #5721, .T. ) ;
#3968 = AXIS2_PLACEMENT_3D ( 'NONE', #6996, #3373, #10359 ) ;
#3969 = ORIENTED_EDGE ( 'NONE', *, *, #10762, .T. ) ;
#3970 = CARTESIAN_POINT ( 'NONE',  ( 30.88479107129467849, 96.16227383530471684, -14.30703002621669562 ) ) ;
#3971 = CARTESIAN_POINT ( 'NONE',  ( 0.000000000000000000, -4.618802153517023612, -3.433295621305388678 ) ) ;
#3972 = AXIS2_PLACEMENT_3D ( 'NONE', #5545, #6742, #4341 ) ;
#3973 = ORIENTED_EDGE ( 'NONE', *, *, #8971, .T. ) ;
#3974 = CARTESIAN_POINT ( 'NONE',  ( 34.62083247296202160, 87.95718916809205723, -13.00000000000000178 ) ) ;
#3975 = VERTEX_POINT ( 'NONE', #14144 ) ;
#3976 = CARTESIAN_POINT ( 'NONE',  ( -42.64958156413675994, -32.39328945492002276, -10.50000000000000000 ) ) ;
#3977 = CARTESIAN_POINT ( 'NONE',  ( 22.33583958711425055, -30.74264578624780597, -25.50000000000000355 ) ) ;
#3978 = VECTOR ( 'NONE', #5191, 1000.000000000000000 ) ;
#3979 = CARTESIAN_POINT ( 'NONE',  ( 0.000000000000000000, 0.000000000000000000, -10.50000000000000000 ) ) ;
#3980 = CARTESIAN_POINT ( 'NONE',  ( 2.100000000000000089, 0.000000000000000000, -5.000000000000000888 ) ) ;
#3981 = DIRECTION ( 'NONE',  ( -1.000000000000000000, 2.682261509073381941E-15, 0.000000000000000000 ) ) ;
#3982 = ADVANCED_FACE ( 'NONE', ( #173 ), #2674, .F. ) ;
#3983 = ORIENTED_EDGE ( 'NONE', *, *, #1243, .T. ) ;
#3984 = EDGE_CURVE ( 'NONE', #1696, #12197, #6848, .T. ) ;
#3985 = DIRECTION ( 'NONE',  ( 0.000000000000000000, 0.000000000000000000, 1.000000000000000000 ) ) ;
#3986 = CARTESIAN_POINT ( 'NONE',  ( 25.00000000000000000, 81.24038404635960831, -31.00000000000000000 ) ) ;
#3987 = UNCERTAINTY_MEASURE_WITH_UNIT (LENGTH_MEASURE( 1.000000000000000082E-05 ), #13732, 'distance_accuracy_value', 'NONE');
#3988 = AXIS2_PLACEMENT_3D ( 'NONE', #12783, #4580, #7141 ) ;
#3989 = LINE ( 'NONE', #13097, #3212 ) ;
#3990 = AXIS2_PLACEMENT_3D ( 'NONE', #5179, #2892, #11253 ) ;
#3991 = AXIS2_PLACEMENT_3D ( 'NONE', #11073, #7712, #11303 ) ;
#3992 = ORIENTED_EDGE ( 'NONE', *, *, #4162, .F. ) ;
#3993 = EDGE_CURVE ( 'NONE', #215, #6594, #6348, .T. ) ;
#3994 = CARTESIAN_POINT ( 'NONE',  ( -36.14014761921588104, 11.74264578624790190, -25.50000000000000355 ) ) ;
#3995 = ORIENTED_EDGE ( 'NONE', *, *, #12207, .F. ) ;
#3996 = CARTESIAN_POINT ( 'NONE',  ( -38.79014761921587251, 11.74264578624790190, 14.49999999999999822 ) ) ;
#3997 = CARTESIAN_POINT ( 'NONE',  ( -11.47770164139309301, 74.11716252799973859, 18.08381726540838486 ) ) ;
#3998 = CIRCLE ( 'NONE', #2778, 60.50000000000000000 ) ;
#3999 = DIRECTION ( 'NONE',  ( 1.000000000000000000, 0.000000000000000000, 0.000000000000000000 ) ) ;
#4000 = CARTESIAN_POINT ( 'NONE',  ( 0.000000000000000000, -4.618802153517023612, -3.433295621305388678 ) ) ;
#4001 = APPLICATION_PROTOCOL_DEFINITION ( 'draft international standard', 'automotive_design', 1998, #12313 ) ;
#4002 = CARTESIAN_POINT ( 'NONE',  ( -51.19406879332065330, -13.71740939043347041, 10.49999999999999822 ) ) ;
#4003 = AXIS2_PLACEMENT_3D ( 'NONE', #223, #9555, #308 ) ;
#4004 = AXIS2_PLACEMENT_3D ( 'NONE', #12435, #2028, #13729 ) ;
#4005 = ORIENTED_EDGE ( 'NONE', *, *, #5698, .T. ) ;
#4006 = ADVANCED_FACE ( 'NONE', ( #7063 ), #1617, .T. ) ;
#4007 = DIRECTION ( 'NONE',  ( -1.000000000000000000, 0.000000000000000000, 0.000000000000000000 ) ) ;
#4008 = CARTESIAN_POINT ( 'NONE',  ( -45.88839665196098849, 26.99988008862674960, -10.50000000000000000 ) ) ;
#4009 = DIRECTION ( 'NONE',  ( 0.000000000000000000, 0.000000000000000000, -1.000000000000000000 ) ) ;
#4010 = VERTEX_POINT ( 'NONE', #2600 ) ;
#4011 = ORIENTED_EDGE ( 'NONE', *, *, #5838, .T. ) ;
#4012 = CYLINDRICAL_SURFACE ( 'NONE', #8584, 63.00000000000000000 ) ;
#4013 = CIRCLE ( 'NONE', #7879, 50.00000000000000000 ) ;
#4014 = ORIENTED_EDGE ( 'NONE', *, *, #4030, .T. ) ;
#4015 = DIRECTION ( 'NONE',  ( 1.000000000000000000, 0.000000000000000000, 0.000000000000000000 ) ) ;
#4016 = CARTESIAN_POINT ( 'NONE',  ( -4.024497503033713564, -2.323544716729502468, -3.572167766733754135 ) ) ;
#4017 = SURFACE_STYLE_USAGE ( .BOTH. , #750 ) ;
#4018 = AXIS2_PLACEMENT_3D ( 'NONE', #4099, #6212, #12149 ) ;
#4019 = DIRECTION ( 'NONE',  ( -0.000000000000000000, -0.000000000000000000, -1.000000000000000000 ) ) ;
#4020 = LINE ( 'NONE', #13278, #10457 ) ;
#4021 = ORIENTED_EDGE ( 'NONE', *, *, #4242, .F. ) ;
#4022 = DIRECTION ( 'NONE',  ( 1.000000000000000000, 0.000000000000000000, 0.000000000000000000 ) ) ;
#4023 = AXIS2_PLACEMENT_3D ( 'NONE', #10094, #7889, #12229 ) ;
#4024 = ORIENTED_EDGE ( 'NONE', *, *, #6547, .F. ) ;
#4025 = B_SPLINE_CURVE_WITH_KNOTS ( 'NONE', 3,
 ( #5486, #5408, #14680, #10109, #11406, #9265, #6910, #10626, #9187, #8131, #4506, #13836, #4647, #6833 ),
 .UNSPECIFIED., .F., .F.,
 ( 4, 2, 2, 2, 2, 2, 4 ),
 ( 0.000000000000000000, 0.001716022237784528602, 0.002574033356676790844, 0.003432044475569052868, 0.004290055594461314459, 0.005148066713353576483, 0.006864088951138102267 ),
 .UNSPECIFIED. ) ;
#4026 = ORIENTED_EDGE ( 'NONE', *, *, #6810, .F. ) ;
#4027 = DIRECTION ( 'NONE',  ( 0.000000000000000000, 0.000000000000000000, 1.000000000000000000 ) ) ;
#4028 = EDGE_CURVE ( 'NONE', #5501, #7998, #13908, .T. ) ;
#4029 = AXIS2_PLACEMENT_3D ( 'NONE', #6873, #10377, #6111 ) ;
#4030 = EDGE_CURVE ( 'NONE', #1777, #14691, #14194, .T. ) ;
#4031 = AXIS2_PLACEMENT_3D ( 'NONE', #2340, #11763, #4775 ) ;
#4032 = CARTESIAN_POINT ( 'NONE',  ( 34.09759333678488247, 101.2734996710205593, -15.50321023462187853 ) ) ;
#4033 = DIRECTION ( 'NONE',  ( 1.000000000000000000, 0.000000000000000000, 0.000000000000000000 ) ) ;
#4034 = DIRECTION ( 'NONE',  ( -1.000000000000000000, 0.000000000000000000, 0.000000000000000000 ) ) ;
#4035 = DIRECTION ( 'NONE',  ( -0.000000000000000000, -0.000000000000000000, 1.000000000000000000 ) ) ;
#4036 = CARTESIAN_POINT ( 'NONE',  ( -2.775557561562891351E-14, -4.618802153517009401, -0.5000000000000004441 ) ) ;
#4037 = ORIENTED_EDGE ( 'NONE', *, *, #7238, .T. ) ;
#4038 = AXIS2_PLACEMENT_3D ( 'NONE', #10815, #415, #10735 ) ;
#4039 = CARTESIAN_POINT ( 'NONE',  ( 2.500000000000002220, 0.000000000000000000, 2.041999999999999815 ) ) ;
#4040 = PRODUCT_DEFINITION_SHAPE ( 'NONE', 'NONE',  #14333 ) ;
#4041 = CARTESIAN_POINT ( 'NONE',  ( 54.55500000000000682, 0.000000000000000000, 2.500000000000000444 ) ) ;
#4042 = PRODUCT_RELATED_PRODUCT_CATEGORY ( 'part', '', ( #11452 ) ) ;
#4043 = CARTESIAN_POINT ( 'NONE',  ( 0.000000000000000000, 0.000000000000000000, 8.000000000000000000 ) ) ;
#4044 = DIRECTION ( 'NONE',  ( -0.000000000000000000, -0.000000000000000000, -1.000000000000000000 ) ) ;
#4045 = EDGE_LOOP ( 'NONE', ( #12281, #7377, #11151, #9153, #6403 ) ) ;
#4046 = LINE ( 'NONE', #11402, #4985 ) ;
#4047 = EDGE_CURVE ( 'NONE', #5260, #13905, #7142, .T. ) ;
#4048 = ORIENTED_EDGE ( 'NONE', *, *, #7590, .T. ) ;
#4049 = DIRECTION ( 'NONE',  ( -1.000000000000000000, 0.000000000000000000, -0.000000000000000000 ) ) ;
#4050 = VERTEX_POINT ( 'NONE', #5032 ) ;
#4051 = CIRCLE ( 'NONE', #14958, 63.00000000000000000 ) ;
#4052 = DIRECTION ( 'NONE',  ( 0.000000000000000000, -0.000000000000000000, 1.000000000000000000 ) ) ;
#4053 = VERTEX_POINT ( 'NONE', #9639 ) ;
#4054 = ORIENTED_EDGE ( 'NONE', *, *, #10702, .T. ) ;
#4055 = CARTESIAN_POINT ( 'NONE',  ( 27.94117647058824616, 90.79807628710781842, -23.50000000000000000 ) ) ;
#4056 = CARTESIAN_POINT ( 'NONE',  ( -51.19406879332065330, -13.71740939043347041, -13.00000000000000178 ) ) ;
#4057 = DIRECTION ( 'NONE',  ( 0.000000000000000000, 0.000000000000000000, 1.000000000000000000 ) ) ;
#4058 = DIRECTION ( 'NONE',  ( 1.000000000000000000, 0.000000000000000000, 0.000000000000000000 ) ) ;
#4059 = CARTESIAN_POINT ( 'NONE',  ( 47.00000000000001421, 81.24038404635960831, -26.00000000000000000 ) ) ;
#4060 = CARTESIAN_POINT ( 'NONE',  ( 50.84834283436990177, 14.07862063237912054, 10.49999999999999822 ) ) ;
#4061 = ORIENTED_EDGE ( 'NONE', *, *, #5695, .F. ) ;
#4062 = CARTESIAN_POINT ( 'NONE',  ( 8.635299310232698033, 74.50321615228340022, -19.90320263233617482 ) ) ;
#4063 = CARTESIAN_POINT ( 'NONE',  ( 0.000000000000000000, 0.000000000000000000, -8.000000000000000000 ) ) ;
#4064 = CARTESIAN_POINT ( 'NONE',  ( 25.00000000000000000, 81.24038404635960831, -23.50000000000000000 ) ) ;
#4065 = PRODUCT_DEFINITION_CONTEXT ( 'detailed design', #2615, 'design' ) ;
#4066 = ORIENTED_EDGE ( 'NONE', *, *, #12665, .F. ) ;
#4067 = CARTESIAN_POINT ( 'NONE',  ( -42.04772703543551415, -32.26435573746212526, -10.50000000000000000 ) ) ;
#4068 = EDGE_CURVE ( 'NONE', #4159, #3184, #4749, .T. ) ;
#4069 = EDGE_CURVE ( 'NONE', #5810, #10576, #8128, .T. ) ;
#4070 = VERTEX_POINT ( 'NONE', #11868 ) ;
#4071 = ADVANCED_FACE ( 'NONE', ( #1461 ), #325, .F. ) ;
#4072 = DIRECTION ( 'NONE',  ( -1.000000000000000000, 0.000000000000000000, 0.000000000000000000 ) ) ;
#4073 = DIRECTION ( 'NONE',  ( 0.000000000000000000, 0.000000000000000000, 1.000000000000000000 ) ) ;
#4074 = CLOSED_SHELL ( 'NONE', ( #8336, #14138, #10257, #10372, #4553, #7136, #597, #835, #8465, #320, #13179, #7400, #960, #11848, #6091, #6800, #220, #2032, #12947, #1976, #9516, #12883, #5963, #10553, #4920, #12024, #9166, #69, #4126, #6176, #3535, #12244, #14526, #10367, #7087, #720, #12936, #4006, #10793, #11373, #12845, #12892, #155, #10610, #5326, #7834, #8116, #5518, #4497, #2875, #10848, #8994, #11217, #1203, #2457, #12532, #13724, #12022, #11169, #9696, #7817, #14483, #6854, #14432, #1800 ) ) ;
#4075 = CARTESIAN_POINT ( 'NONE',  ( 52.72775723226780542, -7.383907457637739036, 10.49999999999999822 ) ) ;
#4076 = FACE_OUTER_BOUND ( 'NONE', #4280, .T. ) ;
#4077 = CARTESIAN_POINT ( 'NONE',  ( -34.13789039812932913, 95.05637002121839885, -16.00000000000000355 ) ) ;
#4078 = ORIENTED_EDGE ( 'NONE', *, *, #8401, .T. ) ;
#4079 = EDGE_CURVE ( 'NONE', #3301, #8551, #14927, .T. ) ;
#4080 = CYLINDRICAL_SURFACE ( 'NONE', #385, 10.00000000000000178 ) ;
#4081 = DIRECTION ( 'NONE',  ( -1.000000000000000000, 1.765157221169382931E-15, 0.000000000000000000 ) ) ;
#4082 = CARTESIAN_POINT ( 'NONE',  ( -68.58935777509570642, -68.58935777509452691, 10.49999999999999822 ) ) ;
#4083 = ORIENTED_EDGE ( 'NONE', *, *, #892, .T. ) ;
#4084 = B_SPLINE_CURVE_WITH_KNOTS ( 'NONE', 3,
 ( #865, #10111, #13601, #10178, #10264, #7826, #705, #14827, #4350, #12471 ),
 .UNSPECIFIED., .F., .F.,
 ( 4, 2, 2, 2, 4 ),
 ( 0.000000000000000000, 0.001708674401391109456, 0.003417348802782218913, 0.005126023204173327935, 0.006834697605564437825 ),
 .UNSPECIFIED. ) ;
#4085 = CIRCLE ( 'NONE', #1893, 2.649999999999989253 ) ;
#4086 = ORIENTED_EDGE ( 'NONE', *, *, #2224, .T. ) ;
#4087 = EDGE_CURVE ( 'NONE', #6876, #836, #12747, .T. ) ;
#4088 = ORIENTED_EDGE ( 'NONE', *, *, #6673, .F. ) ;
#4089 = EDGE_CURVE ( 'NONE', #12422, #6857, #10026, .T. ) ;
#4090 = FACE_OUTER_BOUND ( 'NONE', #7803, .T. ) ;
#4091 = DIRECTION ( 'NONE',  ( -1.000000000000000000, 0.000000000000000000, 0.000000000000000000 ) ) ;
#4092 = ORIENTED_EDGE ( 'NONE', *, *, #15021, .F. ) ;
#4093 = LINE ( 'NONE', #13346, #7530 ) ;
#4094 = CARTESIAN_POINT ( 'NONE',  ( 51.19406879332056093, 13.71740939043382745, -8.000000000000000000 ) ) ;
#4095 = ORIENTED_EDGE ( 'NONE', *, *, #3710, .F. ) ;
#4096 = LINE ( 'NONE', #4178, #1451 ) ;
#4097 = ORIENTED_EDGE ( 'NONE', *, *, #4865, .F. ) ;
#4098 = ORIENTED_EDGE ( 'NONE', *, *, #3365, .T. ) ;
#4099 = CARTESIAN_POINT ( 'NONE',  ( -33.48561063518626923, 47.21331623427104063, 10.49999999999999822 ) ) ;
#4100 = DIRECTION ( 'NONE',  ( 1.000000000000000000, -1.332267629550187849E-14, 0.000000000000000000 ) ) ;
#4101 = DIRECTION ( 'NONE',  ( 0.000000000000000000, 0.000000000000000000, 1.000000000000000000 ) ) ;
#4102 = DIRECTION ( 'NONE',  ( 0.000000000000000000, -1.000000000000000000, 0.000000000000000000 ) ) ;
#4103 = DIRECTION ( 'NONE',  ( 1.000000000000000000, 0.000000000000000000, 0.000000000000000000 ) ) ;
#4104 = CARTESIAN_POINT ( 'NONE',  ( 2.500000000000002220, 0.000000000000000000, 0.000000000000000000 ) ) ;
#4105 = ORIENTED_EDGE ( 'NONE', *, *, #14155, .T. ) ;
#4106 = ADVANCED_FACE ( 'NONE', ( #12385 ), #1111, .T. ) ;
#4107 = CARTESIAN_POINT ( 'NONE',  ( 0.000000000000000000, 0.000000000000000000, -79.80561291909842225 ) ) ;
#4108 = DIRECTION ( 'NONE',  ( 1.000000000000000000, 0.000000000000000000, 0.000000000000000000 ) ) ;
#4109 = CARTESIAN_POINT ( 'NONE',  ( 3.999999999999996447, 2.309401076758511806, -0.5000000000000004441 ) ) ;
#4110 = TOROIDAL_SURFACE ( 'NONE', #8700, 68.00000000000000000, 5.000000000000000000 ) ;
#4111 = CARTESIAN_POINT ( 'NONE',  ( -4.211140560182194292, -2.431303136016555122, -3.745885042887437510 ) ) ;
#4112 = VERTEX_POINT ( 'NONE', #7740 ) ;
#4113 = FACE_OUTER_BOUND ( 'NONE', #9321, .T. ) ;
#4114 = EDGE_LOOP ( 'NONE', ( #7332, #4858, #3950, #4964 ) ) ;
#4115 = CARTESIAN_POINT ( 'NONE',  ( 3.999999999999997335, 1.563622288139205230, -0.2253451193528305807 ) ) ;
#4116 = VERTEX_POINT ( 'NONE', #3125 ) ;
#4117 = CARTESIAN_POINT ( 'NONE',  ( -2.449293598294700991E-16, 97.00000000000000000, 8.000000000000000000 ) ) ;
#4118 =( GEOMETRIC_REPRESENTATION_CONTEXT ( 3 ) GLOBAL_UNCERTAINTY_ASSIGNED_CONTEXT ( ( #10881 ) ) GLOBAL_UNIT_ASSIGNED_CONTEXT ( ( #11982, #12808, #7171 ) ) REPRESENTATION_CONTEXT ( 'NONE', 'WORKASPACE' ) );
#4119 = ORIENTED_EDGE ( 'NONE', *, *, #8284, .F. ) ;
#4120 = CIRCLE ( 'NONE', #4609, 3.000000000000002665 ) ;
#4121 = DIRECTION ( 'NONE',  ( -1.000000000000000000, 0.000000000000000000, 0.000000000000000000 ) ) ;
#4122 = CARTESIAN_POINT ( 'NONE',  ( 33.48561063518626923, -47.21331623427104063, -8.000000000000000000 ) ) ;
#4123 = CARTESIAN_POINT ( 'NONE',  ( -31.74999999999995737, 0.000000000000000000, -2.775557561562891351E-14 ) ) ;
#4124 = AXIS2_PLACEMENT_3D ( 'NONE', #11846, #12982, #13208 ) ;
#4125 = FACE_OUTER_BOUND ( 'NONE', #7137, .T. ) ;
#4126 = ADVANCED_FACE ( 'NONE', ( #4113 ), #6367, .F. ) ;
#4128 = FACE_OUTER_BOUND ( 'NONE', #13282, .T. ) ;
#4127 = CIRCLE ( 'NONE', #6044, 53.55662432702593634 ) ;
#4129 = EDGE_CURVE ( 'NONE', #1495, #13289, #11507, .T. ) ;
#4130 = EDGE_CURVE ( 'NONE', #14448, #10153, #4263, .T. ) ;
#4131 = CARTESIAN_POINT ( 'NONE',  ( -11.92530613726453659, 94.24865542230074311, 17.34466199971670264 ) ) ;
#4132 = ORIENTED_EDGE ( 'NONE', *, *, #10811, .F. ) ;
#4133 = CARTESIAN_POINT ( 'NONE',  ( 8.075966873893682063, 74.56617093413656505, -19.99999999999999645 ) ) ;
#4134 = ORIENTED_EDGE ( 'NONE', *, *, #883, .F. ) ;
#4135 = CARTESIAN_POINT ( 'NONE',  ( 57.06275842387049835, -9.706953719245678514, 10.49999999999999822 ) ) ;
#4136 = CIRCLE ( 'NONE', #14561, 50.00000000000000000 ) ;
#4137 = CARTESIAN_POINT ( 'NONE',  ( 3.999999999999998224, -2.471525695159797031, -3.686886880705772640 ) ) ;
#4138 = AXIS2_PLACEMENT_3D ( 'NONE', #11109, #5418, #2984 ) ;
#4139 = EDGE_CURVE ( 'NONE', #7269, #6876, #7443, .T. ) ;
#4140 = AXIS2_PLACEMENT_3D ( 'NONE', #4812, #3602, #9423 ) ;
#4141 =( GEOMETRIC_REPRESENTATION_CONTEXT ( 3 ) GLOBAL_UNCERTAINTY_ASSIGNED_CONTEXT ( ( #9733 ) ) GLOBAL_UNIT_ASSIGNED_CONTEXT ( ( #518, #7422, #9917 ) ) REPRESENTATION_CONTEXT ( 'NONE', 'WORKASPACE' ) );
#4142 = EDGE_LOOP ( 'NONE', ( #4944, #2690, #4270 ) ) ;
#4143 = CARTESIAN_POINT ( 'NONE',  ( -3.540020015735788395, -2.810662092924504751, -3.602146406945951451 ) ) ;
#4144 = ORIENTED_EDGE ( 'NONE', *, *, #8764, .F. ) ;
#4145 = CARTESIAN_POINT ( 'NONE',  ( 68.58935777509475429, -68.58935777509547904, -8.000000000000000000 ) ) ;
#4146 = CARTESIAN_POINT ( 'NONE',  ( 5.000000000000007105, 85.00000000000000000, 46.00000000000000000 ) ) ;
#4147 = COLOUR_RGB ( '', 0.72549020, 0.75294118, 0.79215686) ;
#4148 = CARTESIAN_POINT ( 'NONE',  ( 7.500000000000000888, 62.55197838597913318, -20.00000000000000000 ) ) ;
#4149 = DIRECTION ( 'NONE',  ( -0.000000000000000000, -0.000000000000000000, -1.000000000000000000 ) ) ;
#4150 = CARTESIAN_POINT ( 'NONE',  ( 0.000000000000000000, 0.000000000000000000, 0.000000000000000000 ) ) ;
#4151 = ORIENTED_EDGE ( 'NONE', *, *, #15022, .F. ) ;
#4152 = CIRCLE ( 'NONE', #4874, 3.000000000000002665 ) ;
#4153 = EDGE_LOOP ( 'NONE', ( #12525, #14322, #3609, #13501 ) ) ;
#4154 = CIRCLE ( 'NONE', #12632, 100.0000000000000000 ) ;
#4155 = DIRECTION ( 'NONE',  ( -1.000000000000000000, 0.000000000000000000, 0.000000000000000000 ) ) ;
#4156 = CYLINDRICAL_SURFACE ( 'NONE', #14999, 60.50000000000000000 ) ;
#4157 = EDGE_CURVE ( 'NONE', #8172, #14105, #1341, .T. ) ;
#4158 = CARTESIAN_POINT ( 'NONE',  ( 27.94117647058824616, 90.79807628710781842, -23.50000000000000000 ) ) ;
#4159 = VERTEX_POINT ( 'NONE', #14599 ) ;
#4160 = VECTOR ( 'NONE', #13756, 1000.000000000000000 ) ;
#4161 = CIRCLE ( 'NONE', #8748, 3.000000000000004441 ) ;
#4162 = EDGE_CURVE ( 'NONE', #5875, #10752, #6907, .T. ) ;
#4163 = ORIENTED_EDGE ( 'NONE', *, *, #9533, .F. ) ;
#4164 = ORIENTED_EDGE ( 'NONE', *, *, #8305, .T. ) ;
#4165 = TOROIDAL_SURFACE ( 'NONE', #13853, 17.00000000000000000, 5.000000000000000000 ) ;
#4166 = ORIENTED_EDGE ( 'NONE', *, *, #10007, .F. ) ;
#4167 = CIRCLE ( 'NONE', #8753, 3.000000000000002665 ) ;
#4168 = DIRECTION ( 'NONE',  ( 1.000000000000000000, 0.000000000000000000, 0.000000000000000000 ) ) ;
#4169 = MANIFOLD_SOLID_BREP ( 'Cut-Extrude1', #8911 ) ;
#4170 = PRODUCT ( 'hex flange nut gradea_iso_ISO - 4161 - M5 - N', 'hex flange nut gradea_iso_ISO - 4161 - M5 - N', '', ( #2927 ) ) ;
#4171 = CARTESIAN_POINT ( 'NONE',  ( 0.000000000000000000, -1.178949249685208533, 2.042000000000002036 ) ) ;
#4172 = SHAPE_REPRESENTATION_RELATIONSHIP ( 'NONE' , 'NONE' ,  #5964, #5117 ) ;
#4173 = DIRECTION ( 'NONE',  ( -0.000000000000000000, -0.000000000000000000, -1.000000000000000000 ) ) ;
#4175 = CIRCLE ( 'NONE', #14847, 3.000000000000002665 ) ;
#4174 = CARTESIAN_POINT ( 'NONE',  ( -9.714003807513870825, -53.63365512954690217, -13.00000000000000178 ) ) ;
#4176 = CARTESIAN_POINT ( 'NONE',  ( -31.76435573746199381, 42.04772703543562073, -10.50000000000000000 ) ) ;
#4177 = ORIENTED_EDGE ( 'NONE', *, *, #7858, .F. ) ;
#4178 = CARTESIAN_POINT ( 'NONE',  ( -2.500000000000000888, 0.000000000000000000, -4.974599999999998801 ) ) ;
#4179 = EDGE_CURVE ( 'NONE', #12800, #8993, #4046, .T. ) ;
#4180 = EDGE_CURVE ( 'NONE', #15011, #9955, #12980, .T. ) ;
#4181 = CIRCLE ( 'NONE', #5387, 3.000000000000002665 ) ;
#4182 = ORIENTED_EDGE ( 'NONE', *, *, #6193, .T. ) ;
#4183 = VERTEX_POINT ( 'NONE', #13761 ) ;
#4184 = CARTESIAN_POINT ( 'NONE',  ( -34.13789339514570287, 95.05636893381519315, 15.99999999999999645 ) ) ;
#4185 = B_SPLINE_CURVE_WITH_KNOTS ( 'NONE', 3,
 ( #9142, #6706, #11356, #11593, #9288 ),
 .UNSPECIFIED., .F., .F.,
 ( 4, 1, 4 ),
 ( 0.000000000000000000, 0.002309401076758506657, 0.004618802153517013315 ),
 .UNSPECIFIED. ) ;
#4186 = CYLINDRICAL_SURFACE ( 'NONE', #7774, 5.000000000000001776 ) ;
#4187 = EDGE_CURVE ( 'NONE', #14140, #362, #7310, .T. ) ;
#4188 = AXIS2_PLACEMENT_3D ( 'NONE', #8301, #8154, #9361 ) ;
#4189 = LINE ( 'NONE', #13438, #11779 ) ;
#4190 = DIRECTION ( 'NONE',  ( 0.000000000000000000, 0.000000000000000000, -1.000000000000000000 ) ) ;
#4191 = DIRECTION ( 'NONE',  ( -0.000000000000000000, -0.000000000000000000, -1.000000000000000000 ) ) ;
#4192 = ORIENTED_EDGE ( 'NONE', *, *, #11689, .F. ) ;
#4193 = FACE_BOUND ( 'NONE', #8365, .T. ) ;
#4194 = VECTOR ( 'NONE', #5045, 1000.000000000000000 ) ;
#4195 = ADVANCED_FACE ( 'NONE', ( #1003 ), #931, .F. ) ;
#4196 = DIRECTION ( 'NONE',  ( -1.000000000000000000, 0.000000000000000000, 0.000000000000000000 ) ) ;
#4197 = DIRECTION ( 'NONE',  ( 0.000000000000000000, 1.471414886128460880E-15, 1.000000000000000000 ) ) ;
#4198 = VERTEX_POINT ( 'NONE', #7819 ) ;
#4199 = ORIENTED_EDGE ( 'NONE', *, *, #4449, .F. ) ;
#4200 = FACE_BOUND ( 'NONE', #461, .T. ) ;
#4201 = ORIENTED_EDGE ( 'NONE', *, *, #3386, .T. ) ;
#4202 = DIRECTION ( 'NONE',  ( 1.000000000000000000, 0.000000000000000000, 0.000000000000000000 ) ) ;
#4203 = ORIENTED_EDGE ( 'NONE', *, *, #1608, .F. ) ;
#4204 = CIRCLE ( 'NONE', #14633, 100.0000000000000000 ) ;
#4205 = VERTEX_POINT ( 'NONE', #9031 ) ;
#4206 = DIRECTION ( 'NONE',  ( 1.000000000000000000, 0.000000000000000000, 0.000000000000000000 ) ) ;
#4207 = FACE_OUTER_BOUND ( 'NONE', #3405, .T. ) ;
#4208 = DIRECTION ( 'NONE',  ( -0.000000000000000000, -0.000000000000000000, 1.000000000000000000 ) ) ;
#4209 = DIRECTION ( 'NONE',  ( -0.000000000000000000, -0.000000000000000000, 1.000000000000000000 ) ) ;
#4210 = FACE_OUTER_BOUND ( 'NONE', #11307, .T. ) ;
#4211 = CARTESIAN_POINT ( 'NONE',  ( 0.000000000000000000, 0.000000000000000000, 13.00000000000000178 ) ) ;
#4212 = CIRCLE ( 'NONE', #8797, 50.00000000000000000 ) ;
#4213 = ORIENTED_EDGE ( 'NONE', *, *, #13274, .T. ) ;
#4214 = CARTESIAN_POINT ( 'NONE',  ( 0.000000000000000000, 0.000000000000000000, -10.50000000000000000 ) ) ;
#4215 = DIRECTION ( 'NONE',  ( 1.000000000000000000, 0.000000000000000000, 0.000000000000000000 ) ) ;
#4216 = AXIS2_PLACEMENT_3D ( 'NONE', #7815, #6675, #14894 ) ;
#4217 = DIRECTION ( 'NONE',  ( -0.000000000000000000, -0.000000000000000000, 1.000000000000000000 ) ) ;
#4218 = EDGE_CURVE ( 'NONE', #5448, #6726, #2803, .T. ) ;
#4219 = ORIENTED_EDGE ( 'NONE', *, *, #10261, .T. ) ;
#4220 = ADVANCED_FACE ( 'NONE', ( #9184 ), #13679, .T. ) ;
#4221 = DIRECTION ( 'NONE',  ( -1.000000000000000000, 0.000000000000000000, 0.000000000000000000 ) ) ;
#4222 = AXIS2_PLACEMENT_3D ( 'NONE', #889, #10130, #10974 ) ;
#4223 = ORIENTED_EDGE ( 'NONE', *, *, #8070, .F. ) ;
#4224 = CARTESIAN_POINT ( 'NONE',  ( 89.61631465359491244, 37.12029293941346708, 8.000000000000000000 ) ) ;
#4225 = CARTESIAN_POINT ( 'NONE',  ( 100.0000000000000000, -3.384287605079545030E-13, -13.00000000000000178 ) ) ;
#4226 = ORIENTED_EDGE ( 'NONE', *, *, #9758, .T. ) ;
#4227 = FACE_OUTER_BOUND ( 'NONE', #14959, .T. ) ;
#4228 = DIRECTION ( 'NONE',  ( -1.000000000000000000, 0.000000000000000000, 0.000000000000000000 ) ) ;
#4229 = CARTESIAN_POINT ( 'NONE',  ( -36.14014761921588104, 11.74264578624790190, -33.00000000000000000 ) ) ;
#4230 = EDGE_LOOP ( 'NONE', ( #5728, #3179, #3312, #11314 ) ) ;
#4231 = EDGE_CURVE ( 'NONE', #15024, #1076, #1590, .T. ) ;
#4232 = ORIENTED_EDGE ( 'NONE', *, *, #12259, .T. ) ;
#4233 = ORIENTED_EDGE ( 'NONE', *, *, #1565, .F. ) ;
#4234 = AXIS2_PLACEMENT_3D ( 'NONE', #3363, #12631, #6847 ) ;
#4235 = DIRECTION ( 'NONE',  ( 0.000000000000000000, 0.000000000000000000, 1.000000000000000000 ) ) ;
#4236 = CARTESIAN_POINT ( 'NONE',  ( 32.10716661655239790, 102.0615849490105376, 13.52016324361725275 ) ) ;
#4237 = CIRCLE ( 'NONE', #5444, 0.5000000000000073275 ) ;
#4238 = ADVANCED_FACE ( 'NONE', ( #2060 ), #11332, .T. ) ;
#4239 = CYLINDRICAL_SURFACE ( 'NONE', #11002, 10.00000000000000178 ) ;
#4240 = ORIENTED_EDGE ( 'NONE', *, *, #3017, .F. ) ;
#4241 = EDGE_LOOP ( 'NONE', ( #10390, #10211, #6704, #8900, #10020 ) ) ;
#4242 = EDGE_CURVE ( 'NONE', #10287, #8196, #11297, .T. ) ;
#4243 = ORIENTED_EDGE ( 'NONE', *, *, #4068, .T. ) ;
#4244 = AXIS2_PLACEMENT_3D ( 'NONE', #6879, #8026, #1139 ) ;
#4245 = DIRECTION ( 'NONE',  ( -0.000000000000000000, -0.000000000000000000, 1.000000000000000000 ) ) ;
#4246 = CIRCLE ( 'NONE', #5927, 63.00000000000000000 ) ;
#4247 = LINE ( 'NONE', #6418, #14638 ) ;
#4248 = CARTESIAN_POINT ( 'NONE',  ( 0.000000000000000000, 0.000000000000000000, -45.50000000000000000 ) ) ;
#4249 = ORIENTED_EDGE ( 'NONE', *, *, #902, .T. ) ;
#4250 = FACE_BOUND ( 'NONE', #1571, .T. ) ;
#4251 = CARTESIAN_POINT ( 'NONE',  ( -31.50188001269984284, 102.2577498558884628, 11.65822132526736432 ) ) ;
#4252 = ORIENTED_EDGE ( 'NONE', *, *, #14625, .T. ) ;
#4253 = DIRECTION ( 'NONE',  ( -0.8191520442889902442, 0.000000000000000000, -0.5735764363510482688 ) ) ;
#4254 = CIRCLE ( 'NONE', #7624, 50.00000000000000000 ) ;
#4255 = AXIS2_PLACEMENT_3D ( 'NONE', #5276, #2086, #9894 ) ;
#4256 = AXIS2_PLACEMENT_3D ( 'NONE', #6938, #8082, #185 ) ;
#4257 = ORIENTED_EDGE ( 'NONE', *, *, #9708, .F. ) ;
#4258 = VECTOR ( 'NONE', #2509, 1000.000000000000227 ) ;
#4259 = ORIENTED_EDGE ( 'NONE', *, *, #5315, .F. ) ;
#4260 = DIRECTION ( 'NONE',  ( -0.000000000000000000, 0.000000000000000000, 1.000000000000000000 ) ) ;
#4261 = DIRECTION ( 'NONE',  ( -1.000000000000000000, 0.000000000000000000, 0.000000000000000000 ) ) ;
#4262 = EDGE_CURVE ( 'NONE', #12963, #1264, #14690, .T. ) ;
#4263 = CIRCLE ( 'NONE', #2061, 3.000000000000002665 ) ;
#4264 = EDGE_CURVE ( 'NONE', #4112, #13996, #7900, .T. ) ;
#4265 = CARTESIAN_POINT ( 'NONE',  ( 2.500000000000002220, 2.357898499370430834, -6.938893903907228378E-15 ) ) ;
#4266 = FACE_OUTER_BOUND ( 'NONE', #8321, .T. ) ;
#4267 = CIRCLE ( 'NONE', #1595, 10.00000000000000178 ) ;
#4268 = FACE_OUTER_BOUND ( 'NONE', #6304, .T. ) ;
#4269 = EDGE_CURVE ( 'NONE', #7351, #1743, #9115, .T. ) ;
#4270 = ORIENTED_EDGE ( 'NONE', *, *, #5483, .F. ) ;
#4271 = DIRECTION ( 'NONE',  ( 0.000000000000000000, 0.000000000000000000, 1.000000000000000000 ) ) ;
#4272 = CIRCLE ( 'NONE', #5710, 3.000000000000002665 ) ;
#4273 = ADVANCED_FACE ( 'NONE', ( #12612 ), #2207, .T. ) ;
#4274 = CARTESIAN_POINT ( 'NONE',  ( 0.000000000000000000, 0.000000000000000000, -20.00000000000000000 ) ) ;
#4275 = DIRECTION ( 'NONE',  ( 0.000000000000000000, 0.000000000000000000, -1.000000000000000000 ) ) ;
#4276 = CIRCLE ( 'NONE', #1126, 59.50000000000000000 ) ;
#4277 = EDGE_LOOP ( 'NONE', ( #2716, #1135 ) ) ;
#4278 = ORIENTED_EDGE ( 'NONE', *, *, #6612, .F. ) ;
#4279 = CARTESIAN_POINT ( 'NONE',  ( 12.39897948556635576, 73.96800191783272282, 16.00000000000000000 ) ) ;
#4280 = EDGE_LOOP ( 'NONE', ( #9167, #14516, #11601, #671 ) ) ;
#4281 = DIRECTION ( 'NONE',  ( 1.000000000000000000, 0.000000000000000000, 0.000000000000000000 ) ) ;
#4282 = ORIENTED_EDGE ( 'NONE', *, *, #7255, .T. ) ;
#4283 = ADVANCED_FACE ( 'NONE', ( #12690 ), #5697, .F. ) ;
#4284 = ORIENTED_EDGE ( 'NONE', *, *, #2023, .F. ) ;
#4285 = FACE_OUTER_BOUND ( 'NONE', #2621, .T. ) ;
#4286 = DIRECTION ( 'NONE',  ( 0.000000000000000000, 0.000000000000000000, 1.000000000000000000 ) ) ;
#4287 = CARTESIAN_POINT ( 'NONE',  ( 20.00000000000000000, 0.000000000000000000, -45.50000000000000000 ) ) ;
#4288 = CIRCLE ( 'NONE', #7661, 0.5000000000000022204 ) ;
#4289 = CYLINDRICAL_SURFACE ( 'NONE', #8000, 3.000000000000002665 ) ;
#4290 = DIRECTION ( 'NONE',  ( 0.000000000000000000, 0.000000000000000000, 1.000000000000000000 ) ) ;
#4291 = CARTESIAN_POINT ( 'NONE',  ( 44.13108361037843252, 56.43380494353993271, -13.00000000000000178 ) ) ;
#4292 = EDGE_LOOP ( 'NONE', ( #13559, #14263 ) ) ;
#4293 = CARTESIAN_POINT ( 'NONE',  ( -7.252293700257136599, -53.06332297728250325, -10.50000000000000000 ) ) ;
#4294 = CARTESIAN_POINT ( 'NONE',  ( -12.50000000000000000, 59.24038404635959409, -20.00000000000000000 ) ) ;
#4295 = CARTESIAN_POINT ( 'NONE',  ( 47.21331623427115431, 33.48561063518610581, -10.50000000000000000 ) ) ;
#4296 = CIRCLE ( 'NONE', #403, 59.50000000000000000 ) ;
#4297 = PRODUCT_DEFINITION_SHAPE ( 'NONE', 'NONE',  #15036 ) ;
#4298 = DIRECTION ( 'NONE',  ( 0.000000000000000000, 0.000000000000000000, -1.000000000000000000 ) ) ;
#4299 = ORIENTED_EDGE ( 'NONE', *, *, #5268, .F. ) ;
#4300 = CARTESIAN_POINT ( 'NONE',  ( -1.390230914382368121, -4.043987460488665420, -3.502507215260525442 ) ) ;
#4301 = ORIENTED_EDGE ( 'NONE', *, *, #13152, .F. ) ;
#4302 = DIRECTION ( 'NONE',  ( 1.000000000000000000, 0.000000000000000000, 0.000000000000000000 ) ) ;
#4303 = FACE_OUTER_BOUND ( 'NONE', #7574, .T. ) ;
#4304 = CARTESIAN_POINT ( 'NONE',  ( 12.46747951117848707, 106.2711918341631900, -15.65812229356676077 ) ) ;
#4305 = LINE ( 'NONE', #7467, #11241 ) ;
#4306 = PRODUCT_CONTEXT ( 'NONE', #9976, 'mechanical' ) ;
#4307 = ORIENTED_EDGE ( 'NONE', *, *, #7924, .F. ) ;
#4308 = ORIENTED_EDGE ( 'NONE', *, *, #1084, .T. ) ;
#4309 = ORIENTED_EDGE ( 'NONE', *, *, #10723, .F. ) ;
#4310 = ADVANCED_FACE ( 'NONE', ( #10402 ), #2287, .T. ) ;
#4311 = DIRECTION ( 'NONE',  ( 0.000000000000000000, 0.000000000000000000, 1.000000000000000000 ) ) ;
#4313 = ADVANCED_FACE ( 'NONE', ( #12769 ), #2353, .T. ) ;
#4312 = LINE ( 'NONE', #1940, #6171 ) ;
#4314 = DIRECTION ( 'NONE',  ( 1.000000000000000000, 0.000000000000000000, 0.000000000000000000 ) ) ;
#4315 = ORIENTED_EDGE ( 'NONE', *, *, #91, .T. ) ;
#4316 = ORIENTED_EDGE ( 'NONE', *, *, #5960, .F. ) ;
#4317 = ORIENTED_EDGE ( 'NONE', *, *, #13624, .F. ) ;
#4318 = CARTESIAN_POINT ( 'NONE',  ( 6.917888187663118416, 52.54657765281190507, 8.000000000000000000 ) ) ;
#4319 = DIRECTION ( 'NONE',  ( 0.000000000000000000, 0.000000000000000000, 1.000000000000000000 ) ) ;
#4320 = SHAPE_REPRESENTATION_RELATIONSHIP ( 'NONE' , 'NONE' ,  #8100, #7823 ) ;
#4321 = DIRECTION ( 'NONE',  ( 0.000000000000000000, 0.000000000000000000, 1.000000000000000000 ) ) ;
#4322 = EDGE_LOOP ( 'NONE', ( #7996, #14796, #7899, #6022 ) ) ;
#4323 = DIRECTION ( 'NONE',  ( 0.000000000000000000, 0.000000000000000000, 1.000000000000000000 ) ) ;
#4324 = CARTESIAN_POINT ( 'NONE',  ( -2.449293598294700991E-16, 97.00000000000000000, -8.000000000000000000 ) ) ;
#4325 = ORIENTED_EDGE ( 'NONE', *, *, #2272, .T. ) ;
#4326 = EDGE_CURVE ( 'NONE', #8856, #10004, #3279, .T. ) ;
#4327 = EDGE_CURVE ( 'NONE', #5762, #13414, #11773, .T. ) ;
#4328 = CARTESIAN_POINT ( 'NONE',  ( -49.00442420935969778, 30.80502811811250297, -10.50000000000000000 ) ) ;
#4329 = EDGE_CURVE ( 'NONE', #2995, #7535, #2079, .T. ) ;
#4330 = ORIENTED_EDGE ( 'NONE', *, *, #4410, .F. ) ;
#4331 = VERTEX_POINT ( 'NONE', #2582 ) ;
#4332 = CARTESIAN_POINT ( 'NONE',  ( -4.211140560182194292, 2.431303136016534250, -3.745885042887433958 ) ) ;
#4333 = ORIENTED_EDGE ( 'NONE', *, *, #9911, .T. ) ;
#4334 = CARTESIAN_POINT ( 'NONE',  ( 7.500000000000000888, 74.62405778299650194, -20.00000000000000000 ) ) ;
#4335 = PLANE ( 'NONE',  #11047 ) ;
#4336 = CARTESIAN_POINT ( 'NONE',  ( -37.12029293941441210, -89.61631465359452875, 10.49999999999999822 ) ) ;
#4337 = CARTESIAN_POINT ( 'NONE',  ( 2.500000000000002220, 1.178949249685208533, -2.042000000000002036 ) ) ;
#4338 = VERTEX_POINT ( 'NONE', #14270 ) ;
#4339 = CIRCLE ( 'NONE', #5056, 53.55662432702593634 ) ;
#4340 = FACE_OUTER_BOUND ( 'NONE', #4898, .T. ) ;
#4341 = DIRECTION ( 'NONE',  ( 1.000000000000000000, 0.000000000000000000, 0.000000000000000000 ) ) ;
#4342 = CARTESIAN_POINT ( 'NONE',  ( 0.000000000000000000, 0.000000000000000000, -10.50000000000000000 ) ) ;
#4343 = EDGE_CURVE ( 'NONE', #10098, #7516, #2549, .T. ) ;
#4344 = ORIENTED_EDGE ( 'NONE', *, *, #1434, .F. ) ;
#4345 = CARTESIAN_POINT ( 'NONE',  ( -33.48561063518626923, 47.21331623427104063, 10.49999999999999822 ) ) ;
#4346 = FACE_BOUND ( 'NONE', #108, .T. ) ;
#4347 = EDGE_CURVE ( 'NONE', #3184, #11976, #4276, .T. ) ;
#4348 = ORIENTED_EDGE ( 'NONE', *, *, #10741, .T. ) ;
#4349 = PLANE ( 'NONE',  #5101 ) ;
#4350 = CARTESIAN_POINT ( 'NONE',  ( -12.28362713749409529, 94.20257980066446635, -16.56510878681792320 ) ) ;
#4351 = CARTESIAN_POINT ( 'NONE',  ( -0.2790467552932288098, -97.41488903138106537, 10.49999999999999822 ) ) ;
#4352 = CARTESIAN_POINT ( 'NONE',  ( 89.33979373934423052, -36.70371619500547666, 10.49999999999999822 ) ) ;
#4353 = EDGE_CURVE ( 'NONE', #2094, #11817, #5480, .T. ) ;
#4354 = DIRECTION ( 'NONE',  ( 1.000000000000000000, 0.000000000000000000, 0.000000000000000000 ) ) ;
#4355 = CARTESIAN_POINT ( 'NONE',  ( 90.11631465359468507, -37.12029293941410657, -13.00000000000000178 ) ) ;
#4356 = DIRECTION ( 'NONE',  ( 1.000000000000000000, 0.000000000000000000, 0.000000000000000000 ) ) ;
#4357 = ORIENTED_EDGE ( 'NONE', *, *, #4600, .T. ) ;
#4358 = CARTESIAN_POINT ( 'NONE',  ( 2.100000000000000089, 0.000000000000000000, -4.694516984716113228 ) ) ;
#4359 = CARTESIAN_POINT ( 'NONE',  ( 10.20439220990035878, 94.45068983291282905, -19.21516791372541988 ) ) ;
#4360 = EDGE_CURVE ( 'NONE', #6631, #197, #8607, .T. ) ;
#4361 = EDGE_CURVE ( 'NONE', #9608, #4909, #14441, .T. ) ;
#4362 = CARTESIAN_POINT ( 'NONE',  ( 4.197310751797290962, 0.8178363989516218568, -3.502498386812445297 ) ) ;
#4363 = AXIS2_PLACEMENT_3D ( 'NONE', #1493, #352, #11752 ) ;
#4364 = DIRECTION ( 'NONE',  ( 1.000000000000000000, 0.000000000000000000, 0.000000000000000000 ) ) ;
#4365 = ORIENTED_EDGE ( 'NONE', *, *, #4416, .F. ) ;
#4366 = CARTESIAN_POINT ( 'NONE',  ( -68.58935777509570642, -68.58935777509452691, -8.000000000000000000 ) ) ;
#4367 = AXIS2_PLACEMENT_3D ( 'NONE', #13667, #8877, #3268 ) ;
#4368 = ORIENTED_EDGE ( 'NONE', *, *, #10013, .T. ) ;
#4369 = CARTESIAN_POINT ( 'NONE',  ( 6.917888187663118416, 52.54657765281190507, -10.50000000000000000 ) ) ;
#4370 = CARTESIAN_POINT ( 'NONE',  ( 0.000000000000000000, 4.618802153517009401, -5.000000000000000888 ) ) ;
#4371 = ADVANCED_FACE ( 'NONE', ( #10478 ), #13986, .T. ) ;
#4372 = ORIENTED_EDGE ( 'NONE', *, *, #2359, .F. ) ;
#4373 = CARTESIAN_POINT ( 'NONE',  ( 11.26223186129995923, 106.4059016791561731, -18.30934846123061632 ) ) ;
#4374 = CARTESIAN_POINT ( 'NONE',  ( -30.80502811811232888, -49.00442420935981147, -10.50000000000000000 ) ) ;
#4375 = APPLICATION_PROTOCOL_DEFINITION ( 'draft international standard', 'automotive_design', 1998, #11945 ) ;
#4376 = EDGE_LOOP ( 'NONE', ( #9697, #237, #1688, #12590 ) ) ;
#4377 = AXIS2_PLACEMENT_3D ( 'NONE', #1884, #12219, #14575 ) ;
#4378 = ORIENTED_EDGE ( 'NONE', *, *, #14291, .T. ) ;
#4379 = VECTOR ( 'NONE', #6548, 1000.000000000000000 ) ;
#4380 = DIRECTION ( 'NONE',  ( 1.000000000000000000, 0.000000000000000000, 0.000000000000000000 ) ) ;
#4381 = CIRCLE ( 'NONE', #3888, 50.00000000000000000 ) ;
#4382 = DIRECTION ( 'NONE',  ( 0.000000000000000000, 1.000000000000000000, -1.471414886128460880E-15 ) ) ;
#4383 = VECTOR ( 'NONE', #8059, 1000.000000000000000 ) ;
#4384 = CARTESIAN_POINT ( 'NONE',  ( 47.21331623427115431, 33.48561063518610581, -13.00000000000000178 ) ) ;
#4385 = ORIENTED_EDGE ( 'NONE', *, *, #3023, .F. ) ;
#4386 = EDGE_LOOP ( 'NONE', ( #11067, #3176, #8706, #2487 ) ) ;
#4387 = ORIENTED_EDGE ( 'NONE', *, *, #2869, .F. ) ;
#4388 = AXIS2_PLACEMENT_3D ( 'NONE', #6352, #9557, #3878 ) ;
#4389 = DIRECTION ( 'NONE',  ( 0.000000000000000000, 0.000000000000000000, 1.000000000000000000 ) ) ;
#4390 = MANIFOLD_SOLID_BREP ( 'EndChamfer', #1885 ) ;
#4391 = CIRCLE ( 'NONE', #12146, 3.000000000000002665 ) ;
#4393 = AXIS2_PLACEMENT_3D ( 'NONE', #1759, #11171, #8882 ) ;
#4392 = DIRECTION ( 'NONE',  ( 1.000000000000000000, 0.000000000000000000, 0.000000000000000000 ) ) ;
#4394 = CARTESIAN_POINT ( 'NONE',  ( 38.79014761921568777, 11.74264578624841171, -25.50000000000000355 ) ) ;
#4395 = CARTESIAN_POINT ( 'NONE',  ( 0.000000000000000000, 0.000000000000000000, 14.49999999999999822 ) ) ;
#4396 = VERTEX_POINT ( 'NONE', #9401 ) ;
#4397 = CYLINDRICAL_SURFACE ( 'NONE', #6556, 3.000000000000002665 ) ;
#4398 = DIRECTION ( 'NONE',  ( 0.000000000000000000, 0.000000000000000000, 1.000000000000000000 ) ) ;
#4399 = ORIENTED_EDGE ( 'NONE', *, *, #13626, .T. ) ;
#4400 = PRESENTATION_LAYER_ASSIGNMENT (  '', '', ( #8495 ) ) ;
#4401 = LINE ( 'NONE', #9011, #2611 ) ;
#4402 = ORIENTED_EDGE ( 'NONE', *, *, #14358, .T. ) ;
#4403 = AXIS2_PLACEMENT_3D ( 'NONE', #10594, #192, #14093 ) ;
#4404 = AXIS2_PLACEMENT_3D ( 'NONE', #5050, #14307, #9737 ) ;
#4405 = ORIENTED_EDGE ( 'NONE', *, *, #13785, .T. ) ;
#4406 = FACE_OUTER_BOUND ( 'NONE', #1195, .T. ) ;
#4407 = EDGE_CURVE ( 'NONE', #8663, #4528, #8380, .T. ) ;
#4408 = EDGE_CURVE ( 'NONE', #10917, #11847, #5147, .T. ) ;
#4409 = ADVANCED_FACE ( 'NONE', ( #6350 ), #10924, .T. ) ;
#4410 = EDGE_CURVE ( 'NONE', #6432, #6463, #2812, .T. ) ;
#4411 = LINE ( 'NONE', #614, #14089 ) ;
#4412 = DIRECTION ( 'NONE',  ( 0.000000000000000000, 0.000000000000000000, 1.000000000000000000 ) ) ;
#4413 = CIRCLE ( 'NONE', #3680, 75.00000000000001421 ) ;
#4414 = DIRECTION ( 'NONE',  ( 0.2941176470588238723, -0.9557692240748189016, 0.000000000000000000 ) ) ;
#4415 = CARTESIAN_POINT ( 'NONE',  ( 2.500000000000002220, -1.768423874527823347, -1.021000000000001018 ) ) ;
#4416 = EDGE_CURVE ( 'NONE', #1158, #11234, #6433, .T. ) ;
#4417 = CARTESIAN_POINT ( 'NONE',  ( 89.61631465359468507, -37.12029293941410657, -10.50000000000000000 ) ) ;
#4418 = AXIS2_PLACEMENT_3D ( 'NONE', #10123, #6541, #4221 ) ;
#4419 = ORIENTED_EDGE ( 'NONE', *, *, #3477, .T. ) ;
#4420 = DIRECTION ( 'NONE',  ( -0.000000000000000000, -0.000000000000000000, -1.000000000000000000 ) ) ;
#4421 = ORIENTED_EDGE ( 'NONE', *, *, #4449, .T. ) ;
#4422 = FACE_OUTER_BOUND ( 'NONE', #2039, .T. ) ;
#4423 = CARTESIAN_POINT ( 'NONE',  ( 4.203833317240876610, 1.627343821129586532, -3.597273115243891262 ) ) ;
#4424 = ORIENTED_EDGE ( 'NONE', *, *, #2993, .T. ) ;
#4425 = CARTESIAN_POINT ( 'NONE',  ( 37.12029293941315444, -89.61631465359504034, -13.00000000000000178 ) ) ;
#4426 = AXIS2_PLACEMENT_3D ( 'NONE', #807, #1926, #6545 ) ;
#4427 = EDGE_CURVE ( 'NONE', #10315, #1158, #10322, .T. ) ;
#4428 = DIRECTION ( 'NONE',  ( -0.000000000000000000, -0.000000000000000000, 1.000000000000000000 ) ) ;
#4429 = CARTESIAN_POINT ( 'NONE',  ( -23.50071946824040836, -45.96504489226015977, 8.000000000000000000 ) ) ;
#4430 = CARTESIAN_POINT ( 'NONE',  ( -12.86891638962156215, 56.43380494353993271, -8.000000000000000000 ) ) ;
#4431 = LINE ( 'NONE', #5332, #9276 ) ;
#4432 = DIRECTION ( 'NONE',  ( -0.000000000000000000, -0.000000000000000000, -1.000000000000000000 ) ) ;
#4433 = EDGE_CURVE ( 'NONE', #6138, #13092, #3294, .T. ) ;
#4434 = DIRECTION ( 'NONE',  ( 0.000000000000000000, 0.000000000000000000, 1.000000000000000000 ) ) ;
#4435 = DIRECTION ( 'NONE',  ( 1.000000000000000000, 0.000000000000000000, 0.000000000000000000 ) ) ;
#4436 = ORIENTED_EDGE ( 'NONE', *, *, #8388, .F. ) ;
#4437 = AXIS2_PLACEMENT_3D ( 'NONE', #11659, #5650, #4525 ) ;
#4438 = DIRECTION ( 'NONE',  ( -0.000000000000000000, -0.000000000000000000, -1.000000000000000000 ) ) ;
#4439 = DIRECTION ( 'NONE',  ( 0.000000000000000000, 0.000000000000000000, 1.000000000000000000 ) ) ;
#4440 = CARTESIAN_POINT ( 'NONE',  ( 30.00000000000000355, 97.48846085563152997, 26.00000000000000000 ) ) ;
#4441 = VERTEX_POINT ( 'NONE', #13507 ) ;
#4442 = DIRECTION ( 'NONE',  ( 0.000000000000000000, 0.000000000000000000, -1.000000000000000000 ) ) ;
#4443 = AXIS2_PLACEMENT_3D ( 'NONE', #6309, #4217, #8827 ) ;
#4444 = ORIENTED_EDGE ( 'NONE', *, *, #13821, .F. ) ;
#4445 = CARTESIAN_POINT ( 'NONE',  ( 2.500000000000002220, -2.357898499370437939, 0.000000000000000000 ) ) ;
#4446 = VERTEX_POINT ( 'NONE', #9854 ) ;
#4447 = DIRECTION ( 'NONE',  ( -0.000000000000000000, -0.000000000000000000, 1.000000000000000000 ) ) ;
#4448 = DIRECTION ( 'NONE',  ( -1.000000000000000000, 0.000000000000000000, 0.000000000000000000 ) ) ;
#4449 = EDGE_CURVE ( 'NONE', #669, #10819, #9822, .T. ) ;
#4450 = AXIS2_PLACEMENT_3D ( 'NONE', #14946, #4763, #14867 ) ;
#4451 = CARTESIAN_POINT ( 'NONE',  ( -49.00442420935969778, 30.80502811811250297, -13.00000000000000178 ) ) ;
#4452 = EDGE_CURVE ( 'NONE', #13716, #6488, #8864, .T. ) ;
#4453 = FACE_OUTER_BOUND ( 'NONE', #8678, .T. ) ;
#4454 = VERTEX_POINT ( 'NONE', #10851 ) ;
#4455 = EDGE_CURVE ( 'NONE', #4704, #8488, #147, .T. ) ;
#4456 = ORIENTED_EDGE ( 'NONE', *, *, #133, .F. ) ;
#4457 = AXIS2_PLACEMENT_3D ( 'NONE', #12126, #12966, #1575 ) ;
#4458 = CARTESIAN_POINT ( 'NONE',  ( 69.08935777509475429, -68.58935777509547904, -10.50000000000000000 ) ) ;
#4459 = CARTESIAN_POINT ( 'NONE',  ( -37.21932736666205699, 89.12622059913296368, -10.50000000000000000 ) ) ;
#4460 = DIRECTION ( 'NONE',  ( -1.000000000000000000, 0.000000000000000000, 0.000000000000000000 ) ) ;
#4461 = EDGE_LOOP ( 'NONE', ( #14666, #6054, #587, #8306 ) ) ;
#4462 = EDGE_CURVE ( 'NONE', #11994, #3488, #1669, .T. ) ;
#4463 = CIRCLE ( 'NONE', #2758, 56.99999999999998579 ) ;
#4464 = ORIENTED_EDGE ( 'NONE', *, *, #2922, .F. ) ;
#4465 = ORIENTED_EDGE ( 'NONE', *, *, #4030, .F. ) ;
#4466 = VECTOR ( 'NONE', #2934, 1000.000000000000000 ) ;
#4467 = CARTESIAN_POINT ( 'NONE',  ( 45.91029614918936375, -26.00011991137331790, -10.50000000000000000 ) ) ;
#4468 = DIRECTION ( 'NONE',  ( 0.000000000000000000, 0.000000000000000000, 1.000000000000000000 ) ) ;
#4469 = EDGE_CURVE ( 'NONE', #14546, #12897, #11118, .T. ) ;
#4470 = CARTESIAN_POINT ( 'NONE',  ( 0.000000000000000000, 0.000000000000000000, 13.00000000000000178 ) ) ;
#4471 = CARTESIAN_POINT ( 'NONE',  ( 0.000000000000000000, 0.000000000000000000, -10.50000000000000000 ) ) ;
#4472 = AXIS2_PLACEMENT_3D ( 'NONE', #8660, #8887, #13521 ) ;
#4473 = CIRCLE ( 'NONE', #6149, 17.00000000000000000 ) ;
#4474 = ORIENTED_EDGE ( 'NONE', *, *, #3014, .F. ) ;
#4475 = DIRECTION ( 'NONE',  ( 1.000000000000000000, 0.000000000000000000, 0.000000000000000000 ) ) ;
#4476 = ORIENTED_EDGE ( 'NONE', *, *, #13230, .F. ) ;
#4477 = CARTESIAN_POINT ( 'NONE',  ( 2.449293598294700991E-16, -97.00000000000000000, -13.00000000000000178 ) ) ;
#4478 = DIRECTION ( 'NONE',  ( 0.000000000000000000, 0.000000000000000000, 1.000000000000000000 ) ) ;
#4479 = VERTEX_POINT ( 'NONE', #14655 ) ;
#4480 = ORIENTED_EDGE ( 'NONE', *, *, #12768, .T. ) ;
#4481 = DIRECTION ( 'NONE',  ( 0.000000000000000000, 0.000000000000000000, 1.000000000000000000 ) ) ;
#4482 = CIRCLE ( 'NONE', #12235, 63.00000000000000000 ) ;
#4483 = TOROIDAL_SURFACE ( 'NONE', #14411, 17.00000000000000000, 5.000000000000000000 ) ;
#4484 = ORIENTED_EDGE ( 'NONE', *, *, #81, .F. ) ;
#4485 = VERTEX_POINT ( 'NONE', #3953 ) ;
#4486 = DIRECTION ( 'NONE',  ( -1.000000000000000000, -1.387778780781434947E-14, 0.000000000000000000 ) ) ;
#4487 = CARTESIAN_POINT ( 'NONE',  ( 9.706953719245472456, 57.06275842387054098, 8.000000000000000000 ) ) ;
#4488 = DIRECTION ( 'NONE',  ( 0.000000000000000000, 0.000000000000000000, 1.000000000000000000 ) ) ;
#4489 = CARTESIAN_POINT ( 'NONE',  ( -33.48561063518626923, 47.21331623427104063, -10.50000000000000000 ) ) ;
#4490 = AXIS2_PLACEMENT_3D ( 'NONE', #11425, #96, #4661 ) ;
#4491 = CARTESIAN_POINT ( 'NONE',  ( -3.492805317593278058, 46.55633131742322917, -10.50000000000000000 ) ) ;
#4492 = EDGE_LOOP ( 'NONE', ( #3057, #12469, #5074, #3734 ) ) ;
#4493 = AXIS2_PLACEMENT_3D ( 'NONE', #6625, #14538, #14848 ) ;
#4494 = AXIS2_PLACEMENT_3D ( 'NONE', #4063, #14158, #6239 ) ;
#4495 = CARTESIAN_POINT ( 'NONE',  ( -3.999999999999996447, -2.309401076758511806, -3.433295621305381573 ) ) ;
#4496 = AXIS2_PLACEMENT_3D ( 'NONE', #11855, #1448, #10783 ) ;
#4497 = ADVANCED_FACE ( 'NONE', ( #3111 ), #13976, .T. ) ;
#4498 = CARTESIAN_POINT ( 'NONE',  ( -4.121772567811602173, -51.45950017607692217, -8.000000000000000000 ) ) ;
#4499 = CARTESIAN_POINT ( 'NONE',  ( -12.86891638962156215, 56.43380494353993271, -10.50000000000000000 ) ) ;
#4500 = EDGE_CURVE ( 'NONE', #1589, #490, #136, .T. ) ;
#4501 = ORIENTED_EDGE ( 'NONE', *, *, #8062, .T. ) ;
#4502 = CARTESIAN_POINT ( 'NONE',  ( -4.203833317240876610, -1.627343821129593415, -3.597273115243891262 ) ) ;
#4503 = AXIS2_PLACEMENT_3D ( 'NONE', #5177, #14515, #9791 ) ;
#4504 = CARTESIAN_POINT ( 'NONE',  ( -51.19406879332065330, -13.71740939043347041, -8.000000000000000000 ) ) ;
#4505 = AXIS2_PLACEMENT_3D ( 'NONE', #6474, #723, #14624 ) ;
#4506 = CARTESIAN_POINT ( 'NONE',  ( -9.442781676091987819, 62.28890912541181990, 19.61600713740890001 ) ) ;
#4507 = AXIS2_PLACEMENT_3D ( 'NONE', #10016, #7808, #2048 ) ;
#4508 = DIRECTION ( 'NONE',  ( 1.000000000000000000, 8.881784197001252323E-16, 0.000000000000000000 ) ) ;
#4509 = DIRECTION ( 'NONE',  ( 0.000000000000000000, 0.000000000000000000, -1.000000000000000000 ) ) ;
#4510 = CARTESIAN_POINT ( 'NONE',  ( 7.500000000000000000, 61.74746958378133144, 20.00000000000000000 ) ) ;
#4511 = DIRECTION ( 'NONE',  ( 0.000000000000000000, 0.000000000000000000, -1.000000000000000000 ) ) ;
#4512 = AXIS2_PLACEMENT_3D ( 'NONE', #1643, #1717, #13263 ) ;
#4513 = AXIS2_PLACEMENT_3D ( 'NONE', #5534, #5753, #839 ) ;
#4514 = VERTEX_POINT ( 'NONE', #7492 ) ;
#4515 = EDGE_CURVE ( 'NONE', #6851, #13058, #5229, .T. ) ;
#4516 = DIRECTION ( 'NONE',  ( -1.000000000000000000, 0.000000000000000000, 0.000000000000000000 ) ) ;
#4517 = CARTESIAN_POINT ( 'NONE',  ( 32.26435573746228158, -42.04772703543541468, 10.49999999999999822 ) ) ;
#4518 = CARTESIAN_POINT ( 'NONE',  ( 3.999999999999996447, -1.539600717839016308, -3.300726591567079371 ) ) ;
#4519 = PLANE ( 'NONE',  #14418 ) ;
#4520 = ORIENTED_EDGE ( 'NONE', *, *, #3225, .T. ) ;
#4521 = AXIS2_PLACEMENT_3D ( 'NONE', #1333, #6172, #5948 ) ;
#4522 = PLANE ( 'NONE',  #35 ) ;
#4523 = VERTEX_POINT ( 'NONE', #14879 ) ;
#4524 = CARTESIAN_POINT ( 'NONE',  ( 35.00000000000000000, 81.24038404635960831, 13.50000000000000533 ) ) ;
#4525 = DIRECTION ( 'NONE',  ( 1.000000000000000000, 0.000000000000000000, 0.000000000000000000 ) ) ;
#4526 = CYLINDRICAL_SURFACE ( 'NONE', #7503, 0.5000000000000004441 ) ;
#4527 = CARTESIAN_POINT ( 'NONE',  ( -49.00442420935969778, 30.80502811811250297, 8.000000000000000000 ) ) ;
#4528 = VERTEX_POINT ( 'NONE', #6884 ) ;
#4529 = ORIENTED_EDGE ( 'NONE', *, *, #14012, .F. ) ;
#4530 = VERTEX_POINT ( 'NONE', #5680 ) ;
#4531 = CIRCLE ( 'NONE', #11070, 53.55662432702593634 ) ;
#4532 = CARTESIAN_POINT ( 'NONE',  ( -51.19406879332065330, -13.71740939043347041, 10.49999999999999822 ) ) ;
#4533 = CARTESIAN_POINT ( 'NONE',  ( 34.51370081393729095, 101.0775402828204363, 15.68973407569667877 ) ) ;
#4534 = CARTESIAN_POINT ( 'NONE',  ( 6.917888187663118416, 52.54657765281190507, -8.000000000000000000 ) ) ;
#4535 = ORIENTED_EDGE ( 'NONE', *, *, #9807, .F. ) ;
#4536 = ADVANCED_FACE ( 'NONE', ( #3185 ), #12591, .F. ) ;
#4537 = EDGE_CURVE ( 'NONE', #14514, #7460, #10555, .T. ) ;
#4538 = ORIENTED_EDGE ( 'NONE', *, *, #2118, .T. ) ;
#4539 = EDGE_LOOP ( 'NONE', ( #6209, #9809, #8776, #8648 ) ) ;
#4540 = AXIS2_PLACEMENT_3D ( 'NONE', #9710, #9945, #13231 ) ;
#4541 = CARTESIAN_POINT ( 'NONE',  ( 0.000000000000000000, 0.000000000000000000, -28.00000000000000000 ) ) ;
#4542 = CYLINDRICAL_SURFACE ( 'NONE', #7041, 2.500000000000000444 ) ;
#4543 = FACE_OUTER_BOUND ( 'NONE', #1515, .T. ) ;
#4544 = FACE_OUTER_BOUND ( 'NONE', #9773, .T. ) ;
#4545 = EDGE_CURVE ( 'NONE', #9298, #8164, #386, .T. ) ;
#4546 = ORIENTED_EDGE ( 'NONE', *, *, #7537, .F. ) ;
#4547 = CARTESIAN_POINT ( 'NONE',  ( 37.12029293941315444, -89.61631465359504034, 10.49999999999999822 ) ) ;
#4548 = ORIENTED_EDGE ( 'NONE', *, *, #539, .F. ) ;
#4549 = CARTESIAN_POINT ( 'NONE',  ( 33.47282819776613394, -39.30189486418255740, -13.00000000000000178 ) ) ;
#4550 = DIRECTION ( 'NONE',  ( 0.000000000000000000, 0.000000000000000000, -1.000000000000000000 ) ) ;
#4551 = EDGE_LOOP ( 'NONE', ( #2096, #9995 ) ) ;
#4552 = EDGE_CURVE ( 'NONE', #8812, #13753, #243, .T. ) ;
#4553 = ADVANCED_FACE ( 'NONE', ( #14734 ), #7651, .T. ) ;
#4554 = ORIENTED_EDGE ( 'NONE', *, *, #13792, .T. ) ;
#4555 = PLANE ( 'NONE',  #12038 ) ;
#4556 = EDGE_LOOP ( 'NONE', ( #11891, #3233, #2776, #9316, #1766, #3206 ) ) ;
#4557 = DIRECTION ( 'NONE',  ( 0.000000000000000000, 0.000000000000000000, -1.000000000000000000 ) ) ;
#4558 = DIRECTION ( 'NONE',  ( 1.000000000000000000, -1.172395514004165559E-13, 0.000000000000000000 ) ) ;
#4559 = CARTESIAN_POINT ( 'NONE',  ( -31.47058823529412663, 102.2673069760056421, 11.00000000000000000 ) ) ;
#4560 = CARTESIAN_POINT ( 'NONE',  ( 0.000000000000000000, 0.000000000000000000, 8.000000000000000000 ) ) ;
#4561 = VERTEX_POINT ( 'NONE', #5605 ) ;
#4562 = VECTOR ( 'NONE', #981, 1000.000000000000000 ) ;
#4563 = DIRECTION ( 'NONE',  ( 1.000000000000000000, 0.000000000000000000, 0.000000000000000000 ) ) ;
#4564 = ORIENTED_EDGE ( 'NONE', *, *, #6462, .T. ) ;
#4565 = DIRECTION ( 'NONE',  ( 1.000000000000000000, 0.000000000000000000, -0.000000000000000000 ) ) ;
#4566 = LINE ( 'NONE', #10400, #3611 ) ;
#4567 = ORIENTED_EDGE ( 'NONE', *, *, #14406, .T. ) ;
#4568 = DIRECTION ( 'NONE',  ( 1.000000000000000000, 0.000000000000000000, 0.000000000000000000 ) ) ;
#4569 = CARTESIAN_POINT ( 'NONE',  ( 32.35455048062397054, 95.67796756487049947, 15.49337032400452863 ) ) ;
#4570 = CIRCLE ( 'NONE', #6725, 75.00000000000001421 ) ;
#4571 = CARTESIAN_POINT ( 'NONE',  ( 0.000000000000000000, 4.862606272033088928, -3.745885042887437510 ) ) ;
#4572 = CARTESIAN_POINT ( 'NONE',  ( 3.349226789952651995, 2.685125164760731487, -0.2236248678334764872 ) ) ;
#4573 = CARTESIAN_POINT ( 'NONE',  ( -12.24154204929785550, 106.2975094407664329, 16.61985167119452811 ) ) ;
#4574 = EDGE_CURVE ( 'NONE', #9479, #8402, #13725, .T. ) ;
#4575 = DIRECTION ( 'NONE',  ( -1.000000000000000000, 0.000000000000000000, 0.000000000000000000 ) ) ;
#4576 = CARTESIAN_POINT ( 'NONE',  ( 2.500000000000002220, -2.357898499370437939, 0.000000000000000000 ) ) ;
#4577 = DIRECTION ( 'NONE',  ( 0.000000000000000000, 0.000000000000000000, 1.000000000000000000 ) ) ;
#4578 = VERTEX_POINT ( 'NONE', #2042 ) ;
#4579 = CARTESIAN_POINT ( 'NONE',  ( 9.714003807514275834, 53.63365512954683112, -8.000000000000000000 ) ) ;
#4580 = DIRECTION ( 'NONE',  ( -0.000000000000000000, -0.000000000000000000, 1.000000000000000000 ) ) ;
#4581 = DIRECTION ( 'NONE',  ( 1.000000000000000000, 0.000000000000000000, -0.000000000000000000 ) ) ;
#4582 = EDGE_LOOP ( 'NONE', ( #2651, #8633, #10326, #3578 ) ) ;
#4583 = DIRECTION ( 'NONE',  ( 1.000000000000000000, 0.000000000000000000, -0.000000000000000000 ) ) ;
#4584 = ORIENTED_EDGE ( 'NONE', *, *, #83, .F. ) ;
#4585 = DIRECTION ( 'NONE',  ( 1.000000000000000000, 0.000000000000000000, 0.000000000000000000 ) ) ;
#4586 = VERTEX_POINT ( 'NONE', #13813 ) ;
#4587 = EDGE_CURVE ( 'NONE', #5511, #3376, #13896, .T. ) ;
#4588 = CARTESIAN_POINT ( 'NONE',  ( 12.39897948556635754, 100.2360479454198696, -16.00000000000000000 ) ) ;
#4589 = EDGE_CURVE ( 'NONE', #10622, #12909, #7411, .T. ) ;
#4590 = CARTESIAN_POINT ( 'NONE',  ( -3.492805317593278058, 46.55633131742322917, -10.50000000000000000 ) ) ;
#4591 = ADVANCED_FACE ( 'NONE', ( #10088 ), #6728, .T. ) ;
#4592 = VECTOR ( 'NONE', #3070, 1000.000000000000000 ) ;
#4593 = DIRECTION ( 'NONE',  ( -0.000000000000000000, -0.000000000000000000, 1.000000000000000000 ) ) ;
#4594 = CARTESIAN_POINT ( 'NONE',  ( -47.21331623427138879, -33.48561063518577896, 8.000000000000000000 ) ) ;
#4595 = ORIENTED_EDGE ( 'NONE', *, *, #14240, .T. ) ;
#4596 = ORIENTED_EDGE ( 'NONE', *, *, #5389, .F. ) ;
#4597 = ORIENTED_EDGE ( 'NONE', *, *, #12291, .T. ) ;
#4598 = ORIENTED_EDGE ( 'NONE', *, *, #7534, .F. ) ;
#4599 = LINE ( 'NONE', #3378, #14948 ) ;
#4600 = EDGE_CURVE ( 'NONE', #12645, #14446, #9583, .T. ) ;
#4601 = PRESENTATION_LAYER_ASSIGNMENT (  '', '', ( #9665 ) ) ;
#4602 = DIRECTION ( 'NONE',  ( -1.000000000000000000, 0.000000000000000000, 0.000000000000000000 ) ) ;
#4603 = CARTESIAN_POINT ( 'NONE',  ( 29.70588235294119173, 96.53269163155674448, 10.99999999999999645 ) ) ;
#4604 = VERTEX_POINT ( 'NONE', #11316 ) ;
#4605 = AXIS2_PLACEMENT_3D ( 'NONE', #1592, #3801, #2726 ) ;
#4606 = EDGE_LOOP ( 'NONE', ( #8119, #935, #437, #393 ) ) ;
#4607 = ORIENTED_EDGE ( 'NONE', *, *, #12597, .T. ) ;
#4608 = CARTESIAN_POINT ( 'NONE',  ( 12.39897948556635576, 73.96800191783272282, 16.00000000000000000 ) ) ;
#4609 = AXIS2_PLACEMENT_3D ( 'NONE', #13349, #8868, #12298 ) ;
#4610 = CARTESIAN_POINT ( 'NONE',  ( -25.00000000000000000, 81.24038404635962252, 31.00000000000000000 ) ) ;
#4611 = DIRECTION ( 'NONE',  ( 0.000000000000000000, 0.000000000000000000, -1.000000000000000000 ) ) ;
#4612 =( LENGTH_UNIT ( ) NAMED_UNIT ( * ) SI_UNIT ( .MILLI., .METRE. ) );
#4613 = AXIS2_PLACEMENT_3D ( 'NONE', #4451, #13478, #9061 ) ;
#4614 = DIRECTION ( 'NONE',  ( 0.000000000000000000, 0.000000000000000000, 1.000000000000000000 ) ) ;
#4615 = AXIS2_PLACEMENT_3D ( 'NONE', #13859, #10426, #3454 ) ;
#4616 = ORIENTED_EDGE ( 'NONE', *, *, #9543, .F. ) ;
#4617 = DIRECTION ( 'NONE',  ( -0.000000000000000000, -0.000000000000000000, -1.000000000000000000 ) ) ;
#4618 = EDGE_CURVE ( 'NONE', #5322, #7158, #12758, .T. ) ;
#4619 = EDGE_LOOP ( 'NONE', ( #7632, #2653, #2338, #15004 ) ) ;
#4620 = CIRCLE ( 'NONE', #12372, 53.55662432702593634 ) ;
#4621 = CARTESIAN_POINT ( 'NONE',  ( 11.55014193876178652, -53.26842454702432406, 8.000000000000000000 ) ) ;
#4622 = DIRECTION ( 'NONE',  ( 0.000000000000000000, 0.000000000000000000, 1.000000000000000000 ) ) ;
#4623 = ORIENTED_EDGE ( 'NONE', *, *, #5000, .F. ) ;
#4624 = ORIENTED_EDGE ( 'NONE', *, *, #733, .F. ) ;
#4625 = DIRECTION ( 'NONE',  ( 0.000000000000000000, 0.000000000000000000, 1.000000000000000000 ) ) ;
#4626 = CIRCLE ( 'NONE', #14578, 100.0000000000000000 ) ;
#4627 = ORIENTED_EDGE ( 'NONE', *, *, #363, .T. ) ;
#4628 = CARTESIAN_POINT ( 'NONE',  ( 47.63108361037843252, 56.43380494353993271, -10.50000000000000000 ) ) ;
#4629 = DIRECTION ( 'NONE',  ( -0.000000000000000000, -0.000000000000000000, 1.000000000000000000 ) ) ;
#4630 = FACE_OUTER_BOUND ( 'NONE', #7313, .T. ) ;
#4631 = CARTESIAN_POINT ( 'NONE',  ( -3.436319922987371989, 2.634841920960311334, -3.531542292954659157 ) ) ;
#4632 = AXIS2_PLACEMENT_3D ( 'NONE', #1296, #7042, #4565 ) ;
#4634 = ORIENTED_EDGE ( 'NONE', *, *, #11236, .F. ) ;
#4633 = ADVANCED_FACE ( 'NONE', ( #10155 ), #4555, .F. ) ;
#4635 = CIRCLE ( 'NONE', #1725, 0.5000000000000038858 ) ;
#4636 = LINE ( 'NONE', #9253, #10656 ) ;
#4637 = ADVANCED_FACE ( 'NONE', ( #4406 ), #1966, .T. ) ;
#4638 = ORIENTED_EDGE ( 'NONE', *, *, #8145, .F. ) ;
#4639 = AXIS2_PLACEMENT_3D ( 'NONE', #1490, #6247, #13260 ) ;
#4640 = CIRCLE ( 'NONE', #9464, 60.50000000000000000 ) ;
#4641 = FACE_OUTER_BOUND ( 'NONE', #11103, .T. ) ;
#4642 = ORIENTED_EDGE ( 'NONE', *, *, #2490, .F. ) ;
#4643 = DIRECTION ( 'NONE',  ( 1.000000000000000000, 0.000000000000000000, 0.000000000000000000 ) ) ;
#4644 = EDGE_CURVE ( 'NONE', #212, #11670, #9348, .T. ) ;
#4645 = CIRCLE ( 'NONE', #9712, 2.649999999999985700 ) ;
#4646 = DIRECTION ( 'NONE',  ( 1.000000000000000000, 0.000000000000000000, 0.000000000000000000 ) ) ;
#4647 = CARTESIAN_POINT ( 'NONE',  ( -8.076099607191862262, 62.48290387921809952, 20.00000000000000000 ) ) ;
#4648 = CARTESIAN_POINT ( 'NONE',  ( 0.000000000000000000, 0.000000000000000000, -23.50000000000000000 ) ) ;
#4649 = CARTESIAN_POINT ( 'NONE',  ( -10.54368182729039738, 106.4795995572428353, 18.98024639174783701 ) ) ;
#4650 = CARTESIAN_POINT ( 'NONE',  ( -1.674280531759317014, 94.51066581171355097, 8.000000000000000000 ) ) ;
#4651 = LINE ( 'NONE', #9124, #1914 ) ;
#4652 = EDGE_CURVE ( 'NONE', #9694, #11315, #2084, .T. ) ;
#4653 = CARTESIAN_POINT ( 'NONE',  ( 0.000000000000000000, 0.000000000000000000, -10.50000000000000000 ) ) ;
#4654 = AXIS2_PLACEMENT_3D ( 'NONE', #9728, #9882, #5192 ) ;
#4655 = EDGE_LOOP ( 'NONE', ( #9559, #1562, #1389, #8757 ) ) ;
#4656 = DIRECTION ( 'NONE',  ( 0.000000000000000000, 0.000000000000000000, -1.000000000000000000 ) ) ;
#4657 = DIRECTION ( 'NONE',  ( 0.000000000000000000, 0.000000000000000000, -1.000000000000000000 ) ) ;
#4658 = CIRCLE ( 'NONE', #5143, 0.5000000000000038858 ) ;
#4659 = CYLINDRICAL_SURFACE ( 'NONE', #14134, 3.000000000000002665 ) ;
#4660 = ORIENTED_EDGE ( 'NONE', *, *, #11960, .T. ) ;
#4661 = DIRECTION ( 'NONE',  ( -1.000000000000000000, 0.000000000000000000, 0.000000000000000000 ) ) ;
#4662 = ORIENTED_EDGE ( 'NONE', *, *, #13578, .F. ) ;
#4663 = CARTESIAN_POINT ( 'NONE',  ( -57.06275842387042729, 9.706953719246069312, -10.50000000000000000 ) ) ;
#4664 = ORIENTED_EDGE ( 'NONE', *, *, #11417, .T. ) ;
#4665 = CIRCLE ( 'NONE', #1509, 50.00000000000000000 ) ;
#4666 = DIRECTION ( 'NONE',  ( -0.000000000000000000, -0.000000000000000000, 1.000000000000000000 ) ) ;
#4667 =( NAMED_UNIT ( * ) SI_UNIT ( $, .STERADIAN. ) SOLID_ANGLE_UNIT ( ) );
#4668 = DIRECTION ( 'NONE',  ( 1.000000000000000000, 8.746504920891462850E-16, 0.000000000000000000 ) ) ;
#4669 = VECTOR ( 'NONE', #6087, 1000.000000000000000 ) ;
#4670 = DIRECTION ( 'NONE',  ( 0.000000000000000000, 0.000000000000000000, -1.000000000000000000 ) ) ;
#4671 = ORIENTED_EDGE ( 'NONE', *, *, #10479, .F. ) ;
#4672 = CYLINDRICAL_SURFACE ( 'NONE', #14710, 63.00000000000000000 ) ;
#4673 = DIRECTION ( 'NONE',  ( 0.000000000000000000, 0.000000000000000000, 1.000000000000000000 ) ) ;
#4674 = CIRCLE ( 'NONE', #3951, 10.00000000000000355 ) ;
#4675 = CARTESIAN_POINT ( 'NONE',  ( -3.999999999999997335, -0.7890432684750902093, -0.04868663549882015773 ) ) ;
#4676 = EDGE_CURVE ( 'NONE', #11699, #13414, #9535, .T. ) ;
#4677 = VERTEX_POINT ( 'NONE', #5005 ) ;
#4678 = EDGE_CURVE ( 'NONE', #11559, #11449, #8331, .T. ) ;
#4679 = AXIS2_PLACEMENT_3D ( 'NONE', #6686, #11340, #1844 ) ;
#4680 = ORIENTED_EDGE ( 'NONE', *, *, #10839, .T. ) ;
#4681 = ORIENTED_EDGE ( 'NONE', *, *, #12795, .F. ) ;
#4682 = DIRECTION ( 'NONE',  ( 0.000000000000000000, 0.000000000000000000, -1.000000000000000000 ) ) ;
#4683 = ADVANCED_FACE ( 'NONE', ( #3631 ), #9609, .F. ) ;
#4684 = CIRCLE ( 'NONE', #7081, 60.50000000000000000 ) ;
#4685 = LINE ( 'NONE', #10664, #13865 ) ;
#4686 = DIRECTION ( 'NONE',  ( 1.000000000000000000, 0.000000000000000000, 0.000000000000000000 ) ) ;
#4687 = PRESENTATION_STYLE_ASSIGNMENT (( #14788 ) ) ;
#4688 = CARTESIAN_POINT ( 'NONE',  ( -96.58511096861892042, -0.2790467552922097916, -10.50000000000000000 ) ) ;
#4689 = ORIENTED_EDGE ( 'NONE', *, *, #11282, .F. ) ;
#4690 = CARTESIAN_POINT ( 'NONE',  ( 22.05882352941176094, 71.68269180561141241, 23.50000000000000355 ) ) ;
#4691 = VECTOR ( 'NONE', #6843, 1000.000000000000000 ) ;
#4692 = ORIENTED_EDGE ( 'NONE', *, *, #3365, .F. ) ;
#4693 = ADVANCED_FACE ( 'NONE', ( #12896 ), #3304, .F. ) ;
#4694 = EDGE_LOOP ( 'NONE', ( #14505, #5457, #12060, #12065, #11607 ) ) ;
#4695 = CARTESIAN_POINT ( 'NONE',  ( -47.21331623427138879, -33.48561063518577896, 8.000000000000000000 ) ) ;
#4696 = DIRECTION ( 'NONE',  ( 0.000000000000000000, 1.000000000000000000, 0.000000000000000000 ) ) ;
#4697 = AXIS2_PLACEMENT_3D ( 'NONE', #5227, #12213, #4091 ) ;
#4698 = EDGE_CURVE ( 'NONE', #11561, #1107, #12517, .T. ) ;
#4699 = ORIENTED_EDGE ( 'NONE', *, *, #12764, .F. ) ;
#4700 = VECTOR ( 'NONE', #8546, 1000.000000000000000 ) ;
#4701 = VERTEX_POINT ( 'NONE', #1362 ) ;
#4702 = DIRECTION ( 'NONE',  ( 0.000000000000000000, 0.000000000000000000, -1.000000000000000000 ) ) ;
#4703 = ORIENTED_EDGE ( 'NONE', *, *, #7162, .F. ) ;
#4704 = VERTEX_POINT ( 'NONE', #11914 ) ;
#4705 = FACE_OUTER_BOUND ( 'NONE', #8778, .T. ) ;
#4706 = DIRECTION ( 'NONE',  ( 0.000000000000000000, 0.000000000000000000, -1.000000000000000000 ) ) ;
#4707 = VECTOR ( 'NONE', #5790, 1000.000000000000000 ) ;
#4708 = CARTESIAN_POINT ( 'NONE',  ( 57.06275842387049835, -9.706953719245678514, -10.50000000000000000 ) ) ;
#4709 = DIRECTION ( 'NONE',  ( 0.000000000000000000, 0.000000000000000000, 1.000000000000000000 ) ) ;
#4710 = CARTESIAN_POINT ( 'NONE',  ( 70.20695371924547601, 57.06275842387054098, -10.50000000000000000 ) ) ;
#4711 = DIRECTION ( 'NONE',  ( -0.000000000000000000, -0.000000000000000000, -1.000000000000000000 ) ) ;
#4712 = ORIENTED_EDGE ( 'NONE', *, *, #4726, .T. ) ;
#4713 = AXIS2_PLACEMENT_3D ( 'NONE', #5102, #14068, #10866 ) ;
#4714 = CIRCLE ( 'NONE', #14409, 50.00000000000000000 ) ;
#4715 = DIRECTION ( 'NONE',  ( 1.000000000000000000, 0.000000000000000000, 0.000000000000000000 ) ) ;
#4716 = CIRCLE ( 'NONE', #12225, 4.999999999999995559 ) ;
#4717 = VERTEX_POINT ( 'NONE', #9387 ) ;
#4718 = SURFACE_STYLE_FILL_AREA ( #76 ) ;
#4719 = EDGE_CURVE ( 'NONE', #12763, #6431, #11692, .T. ) ;
#4720 = ORIENTED_EDGE ( 'NONE', *, *, #4975, .F. ) ;
#4721 = ADVANCED_FACE ( 'NONE', ( #5821 ), #3562, .F. ) ;
#4722 = CARTESIAN_POINT ( 'NONE',  ( 29.70588235294119173, 96.53269163155674448, 10.99999999999999645 ) ) ;
#4723 = EDGE_CURVE ( 'NONE', #12781, #14062, #6642, .T. ) ;
#4724 = ORIENTED_EDGE ( 'NONE', *, *, #14136, .T. ) ;
#4725 = DIRECTION ( 'NONE',  ( 0.000000000000000000, 0.000000000000000000, 1.000000000000000000 ) ) ;
#4726 = EDGE_CURVE ( 'NONE', #12336, #10098, #10781, .T. ) ;
#4727 = CARTESIAN_POINT ( 'NONE',  ( 2.000000000000008882, 3.464101615137750390, 0.000000000000000000 ) ) ;
#4728 = DIRECTION ( 'NONE',  ( 0.000000000000000000, 0.000000000000000000, 1.000000000000000000 ) ) ;
#4729 = DIRECTION ( 'NONE',  ( 1.000000000000000000, 0.000000000000000000, 0.000000000000000000 ) ) ;
#4730 = VECTOR ( 'NONE', #5599, 1000.000000000000000 ) ;
#4731 = AXIS2_PLACEMENT_3D ( 'NONE', #10765, #6200, #10838 ) ;
#4732 = DIRECTION ( 'NONE',  ( 0.000000000000000000, 0.000000000000000000, -1.000000000000000000 ) ) ;
#4733 = ITEM_DEFINED_TRANSFORMATION ( 'NONE', 'NONE', #13084,  #5108 ) ;
#4734 = EDGE_CURVE ( 'NONE', #9852, #4717, #10297, .T. ) ;
#4735 = CYLINDRICAL_SURFACE ( 'NONE', #13876, 2.649999999999992806 ) ;
#4736 = ORIENTED_EDGE ( 'NONE', *, *, #8888, .F. ) ;
#4737 = PLANE ( 'NONE',  #9366 ) ;
#4738 = CARTESIAN_POINT ( 'NONE',  ( -3.349226789952651995, -2.685125164760743033, -0.2236248678334835094 ) ) ;
#4739 = AXIS2_PLACEMENT_3D ( 'NONE', #1684, #10944, #1762 ) ;
#4740 = DIRECTION ( 'NONE',  ( 1.000000000000000000, 0.000000000000000000, 0.000000000000000000 ) ) ;
#4741 = CIRCLE ( 'NONE', #13955, 3.000000000000002665 ) ;
#4742 = CARTESIAN_POINT ( 'NONE',  ( -32.26435573746199736, 42.04772703543562073, -8.000000000000000000 ) ) ;
#4743 = EDGE_CURVE ( 'NONE', #12589, #1338, #2794, .T. ) ;
#4744 = EDGE_LOOP ( 'NONE', ( #7598, #7600, #10772, #14208 ) ) ;
#4745 = CARTESIAN_POINT ( 'NONE',  ( -65.58935777509570642, -68.58935777509452691, -8.000000000000000000 ) ) ;
#4746 = ORIENTED_EDGE ( 'NONE', *, *, #1797, .T. ) ;
#4747 = CARTESIAN_POINT ( 'NONE',  ( -3.999999999999996447, 2.309401076758498039, -0.4999999999999935052 ) ) ;
#4748 = FACE_OUTER_BOUND ( 'NONE', #15010, .T. ) ;
#4749 = CIRCLE ( 'NONE', #5219, 53.55662432702593634 ) ;
#4750 = DIRECTION ( 'NONE',  ( -1.000000000000000000, 0.000000000000000000, 0.000000000000000000 ) ) ;
#4751 = DIRECTION ( 'NONE',  ( -1.000000000000000000, 0.000000000000000000, 0.000000000000000000 ) ) ;
#4752 = CIRCLE ( 'NONE', #13236, 100.0000000000000000 ) ;
#4753 = VERTEX_POINT ( 'NONE', #13970 ) ;
#4754 = CARTESIAN_POINT ( 'NONE',  ( 9.706953719245472456, 57.06275842387054098, -10.50000000000000000 ) ) ;
#4755 = CARTESIAN_POINT ( 'NONE',  ( 25.00000000000000000, 81.24038404635960831, 31.00000000000000000 ) ) ;
#4756 = CARTESIAN_POINT ( 'NONE',  ( 2.500000000000002220, -1.178949249685208533, 2.042000000000002036 ) ) ;
#4757 = AXIS2_PLACEMENT_3D ( 'NONE', #10449, #10305, #8092 ) ;
#4758 = ORIENTED_EDGE ( 'NONE', *, *, #13726, .F. ) ;
#4759 = VERTEX_POINT ( 'NONE', #10536 ) ;
#4760 = VERTEX_POINT ( 'NONE', #7103 ) ;
#4761 = CARTESIAN_POINT ( 'NONE',  ( 7.500000000000000000, 106.7368258849775202, 20.00000000000000355 ) ) ;
#4762 = DIRECTION ( 'NONE',  ( 0.000000000000000000, 0.000000000000000000, -1.000000000000000000 ) ) ;
#4763 = DIRECTION ( 'NONE',  ( 0.000000000000000000, 0.000000000000000000, 1.000000000000000000 ) ) ;
#4764 = EDGE_CURVE ( 'NONE', #6659, #8680, #1578, .T. ) ;
#4765 = DIRECTION ( 'NONE',  ( 1.000000000000000000, 0.000000000000000000, 0.000000000000000000 ) ) ;
#4766 = CIRCLE ( 'NONE', #12282, 60.50000000000000000 ) ;
#4767 = CARTESIAN_POINT ( 'NONE',  ( -9.707422895060656032, 94.50306011459642264, 19.49540453443646726 ) ) ;
#4768 = ORIENTED_EDGE ( 'NONE', *, *, #6043, .F. ) ;
#4769 = ORIENTED_EDGE ( 'NONE', *, *, #2760, .T. ) ;
#4770 = CARTESIAN_POINT ( 'NONE',  ( 3.999999999999996447, 2.309401076758498039, -3.433295621305378020 ) ) ;
#4771 = CARTESIAN_POINT ( 'NONE',  ( 52.05085522212507243, -6.852625091552522640, -10.50000000000000000 ) ) ;
#4772 = LINE ( 'NONE', #11248, #3485 ) ;
#4773 = ORIENTED_EDGE ( 'NONE', *, *, #13256, .T. ) ;
#4774 = ORIENTED_EDGE ( 'NONE', *, *, #9164, .F. ) ;
#4775 = DIRECTION ( 'NONE',  ( 0.000000000000000000, 0.000000000000000000, 1.000000000000000000 ) ) ;
#4776 = ORIENTED_EDGE ( 'NONE', *, *, #8437, .T. ) ;
#4777 = DIRECTION ( 'NONE',  ( -1.000000000000000000, 0.000000000000000000, 0.000000000000000000 ) ) ;
#4778 = CARTESIAN_POINT ( 'NONE',  ( -89.33979373934396051, 36.70371619500605220, 10.49999999999999822 ) ) ;
#4779 = CYLINDRICAL_SURFACE ( 'NONE', #10074, 56.99999999999999289 ) ;
#4780 = DIRECTION ( 'NONE',  ( -1.000000000000000000, 0.000000000000000000, 0.000000000000000000 ) ) ;
#4781 = EDGE_CURVE ( 'NONE', #10988, #6415, #2535, .T. ) ;
#4782 = ADVANCED_FACE ( 'NONE', ( #1427 ), #6036, .T. ) ;
#4783 = DIRECTION ( 'NONE',  ( 0.2941176470588238723, -0.9557692240748189016, 0.000000000000000000 ) ) ;
#4784 = FACE_OUTER_BOUND ( 'NONE', #11618, .T. ) ;
#4785 = ORIENTED_EDGE ( 'NONE', *, *, #11918, .F. ) ;
#4786 = DIRECTION ( 'NONE',  ( 0.000000000000000000, 0.000000000000000000, -1.000000000000000000 ) ) ;
#4787 = VERTEX_POINT ( 'NONE', #13047 ) ;
#4788 = EDGE_LOOP ( 'NONE', ( #6966, #12761, #4680, #13082, #4436 ) ) ;
#4789 = FACE_OUTER_BOUND ( 'NONE', #4461, .T. ) ;
#4790 = ORIENTED_EDGE ( 'NONE', *, *, #2319, .T. ) ;
#4791 = CARTESIAN_POINT ( 'NONE',  ( -56.43380494354004639, -12.86891638962099549, -13.00000000000000178 ) ) ;
#4792 = AXIS2_PLACEMENT_3D ( 'NONE', #10152, #2038, #1755 ) ;
#4793 = DIRECTION ( 'NONE',  ( 1.000000000000000000, 0.000000000000000000, 0.000000000000000000 ) ) ;
#4794 = DIRECTION ( 'NONE',  ( 0.000000000000000000, 0.000000000000000000, 1.000000000000000000 ) ) ;
#4795 = DIRECTION ( 'NONE',  ( -0.000000000000000000, -0.000000000000000000, 1.000000000000000000 ) ) ;
#4796 = CARTESIAN_POINT ( 'NONE',  ( 33.49014761921571903, 11.74264578624841171, 14.49999999999999822 ) ) ;
#4797 = ITEM_DEFINED_TRANSFORMATION ( 'NONE', 'NONE', #14289,  #5108 ) ;
#4798 = CARTESIAN_POINT ( 'NONE',  ( 2.500000000000000888, 3.061616997868384127E-16, -4.974599999999998801 ) ) ;
#4799 = ORIENTED_EDGE ( 'NONE', *, *, #11826, .T. ) ;
#4800 = EDGE_CURVE ( 'NONE', #721, #3540, #858, .T. ) ;
#4801 = B_SPLINE_CURVE_WITH_KNOTS ( 'NONE', 3,
 ( #4770, #13890, #2336, #10530, #134, #10455 ),
 .UNSPECIFIED., .F., .F.,
 ( 4, 2, 4 ),
 ( 0.000000000000000000, 0.0002095117440864783663, 0.0004190234881729567326 ),
 .UNSPECIFIED. ) ;
#4802 = CARTESIAN_POINT ( 'NONE',  ( 0.6448876103708347518, 4.246476118072353145, -0.2256878752776711461 ) ) ;
#4803 = CARTESIAN_POINT ( 'NONE',  ( -68.58935777509570642, -68.58935777509452691, 8.000000000000000000 ) ) ;
#4804 = VECTOR ( 'NONE', #5750, 1000.000000000000000 ) ;
#4805 = EDGE_CURVE ( 'NONE', #7414, #3127, #9076, .T. ) ;
#4806 = DIRECTION ( 'NONE',  ( 1.000000000000000000, 0.000000000000000000, 0.000000000000000000 ) ) ;
#4807 = DIRECTION ( 'NONE',  ( 0.5000000000000022204, 0.8660254037844374864, -0.000000000000000000 ) ) ;
#4808 = ORIENTED_EDGE ( 'NONE', *, *, #13914, .T. ) ;
#4809 = EDGE_CURVE ( 'NONE', #10105, #4879, #10534, .T. ) ;
#4810 = DIRECTION ( 'NONE',  ( 0.000000000000000000, 0.000000000000000000, -1.000000000000000000 ) ) ;
#4811 = ORIENTED_EDGE ( 'NONE', *, *, #8322, .F. ) ;
#4812 = CARTESIAN_POINT ( 'NONE',  ( 57.06275842387049835, -9.706953719245678514, -10.50000000000000000 ) ) ;
#4813 = CARTESIAN_POINT ( 'NONE',  ( 13.60620885621573883, -51.79945067148128146, -10.50000000000000000 ) ) ;
#4814 = CARTESIAN_POINT ( 'NONE',  ( 0.000000000000000000, 0.000000000000000000, -0.3080913168122742518 ) ) ;
#4815 = DIRECTION ( 'NONE',  ( 1.000000000000000000, -8.881784197001252323E-16, 0.000000000000000000 ) ) ;
#4816 = ADVANCED_FACE ( 'NONE', ( #9839 ), #3936, .T. ) ;
#4817 = ORIENTED_EDGE ( 'NONE', *, *, #11886, .T. ) ;
#4818 = EDGE_CURVE ( 'NONE', #11004, #5663, #14183, .T. ) ;
#4819 = CARTESIAN_POINT ( 'NONE',  ( 2.500000000000002220, 2.500728763858895382E-16, -2.041999999999999815 ) ) ;
#4820 = CARTESIAN_POINT ( 'NONE',  ( -14.00000000000000000, 0.000000000000000000, 14.49999999999999822 ) ) ;
#4821 = DIRECTION ( 'NONE',  ( -1.000000000000000000, 0.000000000000000000, 0.000000000000000000 ) ) ;
#4822 = VERTEX_POINT ( 'NONE', #8627 ) ;
#4823 = ORIENTED_EDGE ( 'NONE', *, *, #5340, .F. ) ;
#4824 = EDGE_CURVE ( 'NONE', #7919, #7026, #4254, .T. ) ;
#4825 = ORIENTED_EDGE ( 'NONE', *, *, #7977, .F. ) ;
#4826 = CARTESIAN_POINT ( 'NONE',  ( 12.37198577373457198, 106.2823362334109447, 16.13593661559556480 ) ) ;
#4827 = FACE_OUTER_BOUND ( 'NONE', #8789, .T. ) ;
#4828 = DIRECTION ( 'NONE',  ( 1.000000000000000000, 0.000000000000000000, 0.000000000000000000 ) ) ;
#4829 = DIRECTION ( 'NONE',  ( 0.000000000000000000, 0.000000000000000000, 1.000000000000000000 ) ) ;
#4830 = EDGE_LOOP ( 'NONE', ( #12384, #11292 ) ) ;
#4831 = ORIENTED_EDGE ( 'NONE', *, *, #5960, .T. ) ;
#4832 = VERTEX_POINT ( 'NONE', #14485 ) ;
#4833 = EDGE_LOOP ( 'NONE', ( #12494, #12287, #13338, #9823, #3834, #3375, #3509, #819, #12361 ) ) ;
#4834 = DIRECTION ( 'NONE',  ( -0.000000000000000000, -0.000000000000000000, -1.000000000000000000 ) ) ;
#4835 = AXIS2_PLACEMENT_3D ( 'NONE', #12477, #7686, #2140 ) ;
#4836 = CARTESIAN_POINT ( 'NONE',  ( 86.67575032682076142, 37.71449950291080455, -13.00000000000000178 ) ) ;
#4837 = CARTESIAN_POINT ( 'NONE',  ( 35.00000000000000000, 81.24038404635960831, -23.50000000000000000 ) ) ;
#4838 = ORIENTED_EDGE ( 'NONE', *, *, #1757, .F. ) ;
#4839 = VERTEX_POINT ( 'NONE', #8473 ) ;
#4840 = CARTESIAN_POINT ( 'NONE',  ( 0.000000000000000000, 0.000000000000000000, -8.000000000000000000 ) ) ;
#4841 = EDGE_LOOP ( 'NONE', ( #2980, #5575, #7395, #9349, #10256 ) ) ;
#4842 = CIRCLE ( 'NONE', #13826, 101.0000000000000284 ) ;
#4843 = LINE ( 'NONE', #9465, #13118 ) ;
#4844 = VECTOR ( 'NONE', #2125, 1000.000000000000000 ) ;
#4845 = DIRECTION ( 'NONE',  ( 0.000000000000000000, 0.000000000000000000, 1.000000000000000000 ) ) ;
#4846 = CIRCLE ( 'NONE', #12125, 2.100000000000000089 ) ;
#4847 = CARTESIAN_POINT ( 'NONE',  ( 0.000000000000000000, 0.000000000000000000, -4.484454397937119197 ) ) ;
#4848 = DIRECTION ( 'NONE',  ( 0.000000000000000000, 0.000000000000000000, -1.000000000000000000 ) ) ;
#4849 = ORIENTED_EDGE ( 'NONE', *, *, #2673, .T. ) ;
#4850 = CARTESIAN_POINT ( 'NONE',  ( -12.39897948556635754, 73.96800191783273704, -16.00000000000000000 ) ) ;
#4851 = PLANE ( 'NONE',  #3874 ) ;
#4852 = ORIENTED_EDGE ( 'NONE', *, *, #10378, .F. ) ;
#4853 = PRODUCT_DEFINITION_FORMATION_WITH_SPECIFIED_SOURCE ( 'ANY', '', #11072, .NOT_KNOWN. ) ;
#4854 = CARTESIAN_POINT ( 'NONE',  ( -13.71740939043329277, 51.19406879332069593, -13.00000000000000178 ) ) ;
#4855 = AXIS2_PLACEMENT_3D ( 'NONE', #9698, #2737, #6139 ) ;
#4856 = ORIENTED_EDGE ( 'NONE', *, *, #10490, .T. ) ;
#4857 = AXIS2_PLACEMENT_3D ( 'NONE', #6688, #14830, #7752 ) ;
#4858 = ORIENTED_EDGE ( 'NONE', *, *, #1246, .T. ) ;
#4859 = ADVANCED_FACE ( 'NONE', ( #7333 ), #13272, .F. ) ;
#4860 = AXIS2_PLACEMENT_3D ( 'NONE', #10728, #6164, #13241 ) ;
#4861 = ADVANCED_FACE ( 'NONE', ( #2864 ), #11993, .T. ) ;
#4862 = STYLED_ITEM ( 'NONE', ( #5378 ), #5117 ) ;
#4863 = ORIENTED_EDGE ( 'NONE', *, *, #9991, .F. ) ;
#4864 = SURFACE_SIDE_STYLE ('',( #4718 ) ) ;
#4865 = EDGE_CURVE ( 'NONE', #10615, #3633, #9793, .T. ) ;
#4866 = EDGE_CURVE ( 'NONE', #2406, #7029, #8837, .T. ) ;
#4867 = DIRECTION ( 'NONE',  ( 0.000000000000000000, 0.000000000000000000, -1.000000000000000000 ) ) ;
#4868 = ORIENTED_EDGE ( 'NONE', *, *, #642, .F. ) ;
#4869 = CARTESIAN_POINT ( 'NONE',  ( -12.39897948556635754, 94.18739463280904545, -16.00000000000000000 ) ) ;
#4870 = CIRCLE ( 'NONE', #12617, 22.00000000000001421 ) ;
#4871 = CYLINDRICAL_SURFACE ( 'NONE', #6660, 2.649999999999989253 ) ;
#4872 = PLANE ( 'NONE',  #11424 ) ;
#4873 = DIRECTION ( 'NONE',  ( 1.000000000000000000, 0.000000000000000000, 0.000000000000000000 ) ) ;
#4874 = AXIS2_PLACEMENT_3D ( 'NONE', #2429, #12775, #11577 ) ;
#4875 = CARTESIAN_POINT ( 'NONE',  ( -12.39897948556635754, 100.2360479454198696, 16.00000000000000000 ) ) ;
#4876 = CONTEXT_DEPENDENT_SHAPE_REPRESENTATION ( #14549, #1975 ) ;
#4877 = AXIS2_PLACEMENT_3D ( 'NONE', #9946, #7592, #11020 ) ;
#4878 = CIRCLE ( 'NONE', #10935, 3.000000000000002665 ) ;
#4879 = VERTEX_POINT ( 'NONE', #7839 ) ;
#4880 = CARTESIAN_POINT ( 'NONE',  ( 0.000000000000000000, 0.000000000000000000, -8.000000000000000000 ) ) ;
#4881 = ORIENTED_EDGE ( 'NONE', *, *, #11886, .F. ) ;
#4882 = EDGE_CURVE ( 'NONE', #12788, #3583, #12731, .T. ) ;
#4883 = AXIS2_PLACEMENT_3D ( 'NONE', #6130, #3949, #2807 ) ;
#4884 = DIRECTION ( 'NONE',  ( -1.000000000000000000, 0.000000000000000000, 0.000000000000000000 ) ) ;
#4885 = DIRECTION ( 'NONE',  ( -0.000000000000000000, -0.000000000000000000, -1.000000000000000000 ) ) ;
#4886 = CARTESIAN_POINT ( 'NONE',  ( 4.000000000000000000, -1.062518129035794345E-14, -3.142992957459236791 ) ) ;
#4887 = EDGE_CURVE ( 'NONE', #10576, #10355, #3998, .T. ) ;
#4888 = CIRCLE ( 'NONE', #272, 3.000000000000002665 ) ;
#4889 = DIRECTION ( 'NONE',  ( 1.000000000000000000, 0.000000000000000000, 0.000000000000000000 ) ) ;
#4890 = EDGE_LOOP ( 'NONE', ( #7470, #6289, #13534, #10313, #4785, #1464, #2127, #14316, #13847, #5099, #10398, #4634, #1047, #12613, #1352, #12467, #12222, #14228, #10235, #10739 ) ) ;
#4891 = CARTESIAN_POINT ( 'NONE',  ( -57.06275842387042729, 9.706953719246069312, -13.00000000000000178 ) ) ;
#4892 = ORIENTED_EDGE ( 'NONE', *, *, #6543, .T. ) ;
#4893 = CARTESIAN_POINT ( 'NONE',  ( -22.05882352941176450, 71.68269180561142662, -23.50000000000000000 ) ) ;
#4894 = DIRECTION ( 'NONE',  ( -0.000000000000000000, -0.000000000000000000, 1.000000000000000000 ) ) ;
#4895 = AXIS2_PLACEMENT_3D ( 'NONE', #7485, #8930, #6342 ) ;
#4896 = LINE ( 'NONE', #9507, #14340 ) ;
#4897 = DIRECTION ( 'NONE',  ( 0.000000000000000000, -1.000000000000000000, 0.000000000000000000 ) ) ;
#4898 = EDGE_LOOP ( 'NONE', ( #12021, #6740, #5218, #10990 ) ) ;
#4899 = VECTOR ( 'NONE', #13900, 1000.000000000000000 ) ;
#4900 = DIRECTION ( 'NONE',  ( 0.000000000000000000, 0.000000000000000000, 1.000000000000000000 ) ) ;
#4901 = DIRECTION ( 'NONE',  ( -1.000000000000000000, -1.065814103640150279E-14, 0.000000000000000000 ) ) ;
#4902 = CARTESIAN_POINT ( 'NONE',  ( 34.44830544488820578, 94.94374256356070418, 16.00000000000000000 ) ) ;
#4903 = CIRCLE ( 'NONE', #13620, 3.000000000000002665 ) ;
#4904 = ORIENTED_EDGE ( 'NONE', *, *, #404, .T. ) ;
#4905 = ADVANCED_FACE ( 'NONE', ( #3146 ), #10121, .T. ) ;
#4906 = VERTEX_POINT ( 'NONE', #12491 ) ;
#4907 = ADVANCED_FACE ( 'NONE', ( #2796 ), #6696, .F. ) ;
#4908 = CONICAL_SURFACE ( 'NONE', #6817, 4.000000000000000000, 0.8911886515913786111 ) ;
#4909 = VERTEX_POINT ( 'NONE', #11347 ) ;
#4910 = CARTESIAN_POINT ( 'NONE',  ( 12.46748823216054092, 106.2711901036690705, 15.65608700630148675 ) ) ;
#4911 = EDGE_CURVE ( 'NONE', #6576, #10213, #7415, .T. ) ;
#4912 = EDGE_CURVE ( 'NONE', #508, #2772, #4976, .T. ) ;
#4913 = DIRECTION ( 'NONE',  ( 0.000000000000000000, 0.000000000000000000, 1.000000000000000000 ) ) ;
#4914 = CARTESIAN_POINT ( 'NONE',  ( 1.390230914382202032, 4.043987460488489560, -3.502507215260438844 ) ) ;
#4915 =( NAMED_UNIT ( * ) PLANE_ANGLE_UNIT ( ) SI_UNIT ( $, .RADIAN. ) );
#4916 = CARTESIAN_POINT ( 'NONE',  ( 18.52941176470587692, 60.21346111671358159, 16.00000000000000000 ) ) ;
#4917 = ORIENTED_EDGE ( 'NONE', *, *, #12475, .F. ) ;
#4918 = CIRCLE ( 'NONE', #801, 10.00000000000000355 ) ;
#4919 = VERTEX_POINT ( 'NONE', #5145 ) ;
#4920 = ADVANCED_FACE ( 'NONE', ( #14404 ), #4012, .F. ) ;
#4921 = CARTESIAN_POINT ( 'NONE',  ( 0.2790467552932288098, 97.41488903138106537, -13.00000000000000178 ) ) ;
#4922 = CARTESIAN_POINT ( 'NONE',  ( 7.500000000000000000, 59.24038404635959409, 15.00000000000000000 ) ) ;
#4923 = AXIS2_PLACEMENT_3D ( 'NONE', #12099, #14151, #10644 ) ;
#4924 = LINE ( 'NONE', #505, #4700 ) ;
#4925 = ORIENTED_EDGE ( 'NONE', *, *, #2501, .F. ) ;
#4926 = ORIENTED_EDGE ( 'NONE', *, *, #6700, .F. ) ;
#4927 = DIRECTION ( 'NONE',  ( -1.000000000000000000, 2.678169576946649542E-15, 0.000000000000000000 ) ) ;
#4928 = ORIENTED_EDGE ( 'NONE', *, *, #5776, .T. ) ;
#4929 = VECTOR ( 'NONE', #10573, 1000.000000000000000 ) ;
#4930 = ADVANCED_FACE ( 'NONE', ( #11724 ), #8147, .T. ) ;
#4931 = CARTESIAN_POINT ( 'NONE',  ( -7.500000000000000888, 59.24038404635959409, -15.00000000000000000 ) ) ;
#4932 = CARTESIAN_POINT ( 'NONE',  ( 5.204748896376250896E-15, 85.00000000000000000, 46.00000000000000000 ) ) ;
#4933 = CARTESIAN_POINT ( 'NONE',  ( 0.000000000000000000, 0.000000000000000000, -26.00000000000000000 ) ) ;
#4934 = ORIENTED_EDGE ( 'NONE', *, *, #7601, .F. ) ;
#4935 = AXIS2_PLACEMENT_3D ( 'NONE', #13548, #5508, #4228 ) ;
#4936 = LINE ( 'NONE', #5230, #8270 ) ;
#4937 = CARTESIAN_POINT ( 'NONE',  ( 47.00000000000001421, 81.24038404635960831, 26.00000000000000000 ) ) ;
#4938 = EDGE_LOOP ( 'NONE', ( #7193, #13086, #11703, #8686 ) ) ;
#4939 = DIRECTION ( 'NONE',  ( 0.000000000000000000, 0.000000000000000000, 1.000000000000000000 ) ) ;
#4940 = CIRCLE ( 'NONE', #4457, 3.000000000000002665 ) ;
#4941 = ORIENTED_EDGE ( 'NONE', *, *, #2793, .T. ) ;
#4942 = ORIENTED_EDGE ( 'NONE', *, *, #15022, .T. ) ;
#4943 = CARTESIAN_POINT ( 'NONE',  ( -26.49999999999971578, -45.89934640057541060, -13.00000000000000178 ) ) ;
#4944 = ORIENTED_EDGE ( 'NONE', *, *, #5559, .F. ) ;
#4945 = AXIS2_PLACEMENT_3D ( 'NONE', #14773, #14542, #6628 ) ;
#4946 = CARTESIAN_POINT ( 'NONE',  ( 68.01302780753354682, -65.64523757230297463, 8.000000000000000000 ) ) ;
#4947 = CARTESIAN_POINT ( 'NONE',  ( 36.14014761921570340, 11.74264578624841171, -25.50000000000000355 ) ) ;
#4948 = DIRECTION ( 'NONE',  ( -1.000000000000000000, 0.000000000000000000, 0.000000000000000000 ) ) ;
#4949 = DIRECTION ( 'NONE',  ( -0.000000000000000000, -0.000000000000000000, 1.000000000000000000 ) ) ;
#4950 = FACE_OUTER_BOUND ( 'NONE', #2809, .T. ) ;
#4951 = DIRECTION ( 'NONE',  ( 0.000000000000000000, 0.000000000000000000, 1.000000000000000000 ) ) ;
#4952 = ORIENTED_EDGE ( 'NONE', *, *, #11227, .T. ) ;
#4953 = CIRCLE ( 'NONE', #2524, 22.00000000000000355 ) ;
#4954 = ADVANCED_FACE ( 'NONE', ( #1317 ), #3597, .F. ) ;
#4955 = AXIS2_PLACEMENT_3D ( 'NONE', #10276, #13777, #5717 ) ;
#4956 = LINE ( 'NONE', #4039, #8729 ) ;
#4957 = EDGE_CURVE ( 'NONE', #7149, #14223, #7383, .T. ) ;
#4958 = VECTOR ( 'NONE', #7522, 1000.000000000000000 ) ;
#4959 = ORIENTED_EDGE ( 'NONE', *, *, #8001, .T. ) ;
#4960 = CARTESIAN_POINT ( 'NONE',  ( 45.89934640057532533, -26.49999999999987566, -8.000000000000000000 ) ) ;
#4961 = DIRECTION ( 'NONE',  ( 0.000000000000000000, 0.000000000000000000, 1.000000000000000000 ) ) ;
#4962 = CARTESIAN_POINT ( 'NONE',  ( -41.54772703543551415, -32.26435573746212526, -13.00000000000000178 ) ) ;
#4963 = CARTESIAN_POINT ( 'NONE',  ( -3.999999999999996447, -2.309401076758511806, -3.433295621305381573 ) ) ;
#4964 = ORIENTED_EDGE ( 'NONE', *, *, #5737, .F. ) ;
#4965 = AXIS2_PLACEMENT_3D ( 'NONE', #13807, #3401, #13965 ) ;
#4966 = CARTESIAN_POINT ( 'NONE',  ( 4.207491450040565795, -2.029819825146484735, -3.671670828759566962 ) ) ;
#4967 = AXIS2_PLACEMENT_3D ( 'NONE', #13956, #13642, #3550 ) ;
#4968 = ORIENTED_EDGE ( 'NONE', *, *, #8110, .T. ) ;
#4969 = EDGE_CURVE ( 'NONE', #8885, #10986, #13697, .T. ) ;
#4970 = FACE_BOUND ( 'NONE', #5840, .T. ) ;
#4971 = DIRECTION ( 'NONE',  ( 1.000000000000000000, 0.000000000000000000, 0.000000000000000000 ) ) ;
#4972 = CARTESIAN_POINT ( 'NONE',  ( -31.62605012285503392, 102.2189371620064691, -12.30800327571618347 ) ) ;
#4973 = DIRECTION ( 'NONE',  ( 0.000000000000000000, 0.000000000000000000, 1.000000000000000000 ) ) ;
#4974 = ADVANCED_FACE ( 'NONE', ( #5782 ), #4519, .F. ) ;
#4975 = EDGE_CURVE ( 'NONE', #511, #14, #12785, .T. ) ;
#4976 = CIRCLE ( 'NONE', #11270, 22.00000000000000000 ) ;
#4977 = VERTEX_POINT ( 'NONE', #11586 ) ;
#4978 = AXIS2_PLACEMENT_3D ( 'NONE', #655, #423, #2849 ) ;
#4979 = FACE_BOUND ( 'NONE', #14570, .T. ) ;
#4980 = DIRECTION ( 'NONE',  ( 1.000000000000000000, 0.000000000000000000, -0.000000000000000000 ) ) ;
#4981 = AXIS2_PLACEMENT_3D ( 'NONE', #10338, #1383, #10627 ) ;
#4982 = DIRECTION ( 'NONE',  ( 1.000000000000000000, 0.000000000000000000, 0.000000000000000000 ) ) ;
#4983 = ORIENTED_EDGE ( 'NONE', *, *, #11746, .F. ) ;
#4984 = FACE_OUTER_BOUND ( 'NONE', #8296, .T. ) ;
#4985 = VECTOR ( 'NONE', #11569, 1000.000000000000000 ) ;
#4986 = ORIENTED_EDGE ( 'NONE', *, *, #8299, .T. ) ;
#4987 = DIRECTION ( 'NONE',  ( 0.000000000000000000, 0.000000000000000000, 1.000000000000000000 ) ) ;
#4988 = CIRCLE ( 'NONE', #581, 60.50000000000000000 ) ;
#4989 = VECTOR ( 'NONE', #922, 1000.000000000000000 ) ;
#4990 = DIRECTION ( 'NONE',  ( 0.000000000000000000, 0.000000000000000000, 1.000000000000000000 ) ) ;
#4991 = CARTESIAN_POINT ( 'NONE',  ( -69.08004447556112382, -68.68541276968802833, -10.50000000000000000 ) ) ;
#4992 = CARTESIAN_POINT ( 'NONE',  ( -22.05882352941176450, 71.68269180561142662, 13.50000000000000533 ) ) ;
#4993 = ORIENTED_EDGE ( 'NONE', *, *, #12309, .F. ) ;
#4994 = ORIENTED_EDGE ( 'NONE', *, *, #12616, .F. ) ;
#4996 = ORIENTED_EDGE ( 'NONE', *, *, #4187, .T. ) ;
#4995 = VECTOR ( 'NONE', #3781, 1000.000000000000000 ) ;
#4997 = CARTESIAN_POINT ( 'NONE',  ( -36.62029293941440500, -89.61631465359452875, -13.00000000000000178 ) ) ;
#4998 = CYLINDRICAL_SURFACE ( 'NONE', #12012, 0.5000000000000004441 ) ;
#4999 = AXIS2_PLACEMENT_3D ( 'NONE', #9554, #12010, #11781 ) ;
#5000 = EDGE_CURVE ( 'NONE', #12796, #219, #7861, .T. ) ;
#5001 = LINE ( 'NONE', #13041, #2027 ) ;
#5002 = VERTEX_POINT ( 'NONE', #21 ) ;
#5003 = EDGE_CURVE ( 'NONE', #6857, #9519, #1330, .T. ) ;
#5004 = EDGE_LOOP ( 'NONE', ( #14853, #1986, #11655, #44, #4315 ) ) ;
#5005 = CARTESIAN_POINT ( 'NONE',  ( -89.33979373934396051, 36.70371619500605220, -10.50000000000000000 ) ) ;
#5006 = EDGE_LOOP ( 'NONE', ( #6244, #9510, #13738, #4424 ) ) ;
#5007 = CIRCLE ( 'NONE', #1374, 0.5000000000000022204 ) ;
#5008 = CARTESIAN_POINT ( 'NONE',  ( -37.12029293941441210, -89.61631465359452875, 8.000000000000000000 ) ) ;
#5009 = EDGE_CURVE ( 'NONE', #6265, #7513, #605, .T. ) ;
#5010 = CARTESIAN_POINT ( 'NONE',  ( -0.1404048886732822965, -4.699864953788087441, -3.686887068327046268 ) ) ;
#5011 = CARTESIAN_POINT ( 'NONE',  ( 23.50071946824040836, 45.96504489226015977, 8.000000000000000000 ) ) ;
#5012 = CARTESIAN_POINT ( 'NONE',  ( 30.80502811811196295, 49.00442420936003174, -13.00000000000000178 ) ) ;
#5013 = DIRECTION ( 'NONE',  ( 1.000000000000000000, 0.000000000000000000, 0.000000000000000000 ) ) ;
#5014 = ORIENTED_EDGE ( 'NONE', *, *, #7200, .F. ) ;
#5015 = FACE_OUTER_BOUND ( 'NONE', #8179, .T. ) ;
#5016 = EDGE_CURVE ( 'NONE', #7285, #11296, #12245, .T. ) ;
#5017 = EDGE_CURVE ( 'NONE', #3376, #14898, #14915, .T. ) ;
#5018 = AXIS2_PLACEMENT_3D ( 'NONE', #9130, #1019, #2075 ) ;
#5019 = EDGE_LOOP ( 'NONE', ( #1039, #1546 ) ) ;
#5020 = ORIENTED_EDGE ( 'NONE', *, *, #11048, .T. ) ;
#5021 = DIRECTION ( 'NONE',  ( -1.000000000000000000, 0.000000000000000000, 0.000000000000000000 ) ) ;
#5022 = VERTEX_POINT ( 'NONE', #10497 ) ;
#5023 = DIRECTION ( 'NONE',  ( 0.000000000000000000, 0.000000000000000000, 1.000000000000000000 ) ) ;
#5024 = FACE_OUTER_BOUND ( 'NONE', #739, .T. ) ;
#5025 = LINE ( 'NONE', #1604, #747 ) ;
#5026 = CARTESIAN_POINT ( 'NONE',  ( 0.3208286057739611619, -4.433571671609693787, -0.3503314178412661462 ) ) ;
#5027 = PLANE ( 'NONE',  #6021 ) ;
#5028 = ORIENTED_EDGE ( 'NONE', *, *, #11695, .T. ) ;
#5029 = EDGE_LOOP ( 'NONE', ( #9634, #3151 ) ) ;
#5030 = CARTESIAN_POINT ( 'NONE',  ( -11.26445476358325237, 106.4056658731563942, -18.30680964731275040 ) ) ;
#5031 = FACE_OUTER_BOUND ( 'NONE', #7936, .T. ) ;
#5032 = CARTESIAN_POINT ( 'NONE',  ( 2.500000000000002220, -1.178949249685208533, 2.042000000000002036 ) ) ;
#5033 = CARTESIAN_POINT ( 'NONE',  ( 9.706953719245472456, 57.06275842387054098, 10.49999999999999822 ) ) ;
#5034 = ORIENTED_EDGE ( 'NONE', *, *, #8593, .T. ) ;
#5035 = DIRECTION ( 'NONE',  ( 0.000000000000000000, 0.000000000000000000, -1.000000000000000000 ) ) ;
#5036 = ORIENTED_EDGE ( 'NONE', *, *, #883, .T. ) ;
#5037 = CARTESIAN_POINT ( 'NONE',  ( -39.04772703543551415, -32.26435573746212526, -8.000000000000000000 ) ) ;
#5038 = DIRECTION ( 'NONE',  ( -0.000000000000000000, -0.000000000000000000, 1.000000000000000000 ) ) ;
#5039 = DIRECTION ( 'NONE',  ( 1.000000000000000000, 0.000000000000000000, 0.000000000000000000 ) ) ;
#5040 = DIRECTION ( 'NONE',  ( -1.000000000000000000, 0.000000000000000000, 0.000000000000000000 ) ) ;
#5041 = CARTESIAN_POINT ( 'NONE',  ( -8.915162460657663601, 94.58113943660329426, 19.80393736615727462 ) ) ;
#5042 = ORIENTED_EDGE ( 'NONE', *, *, #1167, .T. ) ;
#5043 = FACE_OUTER_BOUND ( 'NONE', #7556, .T. ) ;
#5044 = CARTESIAN_POINT ( 'NONE',  ( 0.000000000000000000, 0.000000000000000000, -25.50000000000000355 ) ) ;
#5045 = DIRECTION ( 'NONE',  ( -0.000000000000000000, -1.000000000000000000, -0.000000000000000000 ) ) ;
#5046 = EDGE_CURVE ( 'NONE', #13753, #13650, #9355, .T. ) ;
#5047 = ORIENTED_EDGE ( 'NONE', *, *, #12369, .T. ) ;
#5048 = ADVANCED_FACE ( 'NONE', ( #12851 ), #9134, .T. ) ;
#5049 = EDGE_CURVE ( 'NONE', #2937, #5169, #7064, .T. ) ;
#5050 = CARTESIAN_POINT ( 'NONE',  ( 51.19406879332056093, 13.71740939043382745, -10.50000000000000000 ) ) ;
#5051 = ORIENTED_EDGE ( 'NONE', *, *, #14652, .T. ) ;
#5052 = CARTESIAN_POINT ( 'NONE',  ( -65.64523757230321621, -68.01302780753330524, 8.000000000000000000 ) ) ;
#5053 = CARTESIAN_POINT ( 'NONE',  ( 12.07377633196514211, 61.83297368684233675, -17.10072941380095202 ) ) ;
#5054 = CARTESIAN_POINT ( 'NONE',  ( -0.1410422978106116165, 4.700232962125094005, -3.687027686973625151 ) ) ;
#5055 = CARTESIAN_POINT ( 'NONE',  ( 30.43807145043610518, -39.66766701456170097, -8.000000000000000000 ) ) ;
#5056 = AXIS2_PLACEMENT_3D ( 'NONE', #5764, #11399, #13984 ) ;
#5057 = VERTEX_POINT ( 'NONE', #6762 ) ;
#5058 = ORIENTED_EDGE ( 'NONE', *, *, #4433, .F. ) ;
#5059 = FACE_OUTER_BOUND ( 'NONE', #5765, .T. ) ;
#5060 = DIRECTION ( 'NONE',  ( -0.000000000000000000, -0.000000000000000000, 1.000000000000000000 ) ) ;
#5061 = CARTESIAN_POINT ( 'NONE',  ( 2.500000000000002220, -1.768423874527823347, 1.021000000000001018 ) ) ;
#5062 = VERTEX_POINT ( 'NONE', #5642 ) ;
#5063 = ORIENTED_EDGE ( 'NONE', *, *, #1707, .T. ) ;
#5064 = DIRECTION ( 'NONE',  ( 0.000000000000000000, 0.000000000000000000, 1.000000000000000000 ) ) ;
#5065 = ORIENTED_EDGE ( 'NONE', *, *, #8327, .F. ) ;
#5066 = FACE_OUTER_BOUND ( 'NONE', #11729, .T. ) ;
#5067 = EDGE_CURVE ( 'NONE', #1787, #10362, #12711, .T. ) ;
#5068 = LINE ( 'NONE', #6261, #12474 ) ;
#5069 = FILL_AREA_STYLE ('',( #440 ) ) ;
#5070 = AXIS2_PLACEMENT_3D ( 'NONE', #9960, #6460, #8821 ) ;
#5071 = EDGE_LOOP ( 'NONE', ( #1142, #12074 ) ) ;
#5072 = CARTESIAN_POINT ( 'NONE',  ( -4.999999999999996447, 85.00000000000000000, 46.00000000000000000 ) ) ;
#5073 = CARTESIAN_POINT ( 'NONE',  ( 0.000000000000000000, 0.000000000000000000, 14.49999999999999822 ) ) ;
#5074 = ORIENTED_EDGE ( 'NONE', *, *, #5337, .T. ) ;
#5075 = CARTESIAN_POINT ( 'NONE',  ( -92.38795325112825196, 38.26834323651002023, -8.000000000000000000 ) ) ;
#5076 = ORIENTED_EDGE ( 'NONE', *, *, #14627, .F. ) ;
#5077 = STYLED_ITEM ( 'NONE', ( #12881 ), #1675 ) ;
#5078 = ORIENTED_EDGE ( 'NONE', *, *, #12338, .F. ) ;
#5079 = CARTESIAN_POINT ( 'NONE',  ( -29.73684948645749415, 96.52317830260923870, 11.65681975620353938 ) ) ;
#5080 = AXIS2_PLACEMENT_3D ( 'NONE', #6128, #10693, #5013 ) ;
#5081 = DIRECTION ( 'NONE',  ( 0.000000000000000000, 0.000000000000000000, -1.000000000000000000 ) ) ;
#5082 = EDGE_CURVE ( 'NONE', #5248, #9892, #12224, .T. ) ;
#5083 = EDGE_CURVE ( 'NONE', #6523, #628, #1463, .T. ) ;
#5084 = DIRECTION ( 'NONE',  ( 1.000000000000000000, -0.000000000000000000, -0.000000000000000000 ) ) ;
#5085 = CARTESIAN_POINT ( 'NONE',  ( 7.500000000000007105, 85.00000000000000000, 31.00000000000000000 ) ) ;
#5086 = CARTESIAN_POINT ( 'NONE',  ( 52.54657765281197612, -6.917888187662545540, -8.000000000000000000 ) ) ;
#5087 = VECTOR ( 'NONE', #12170, 1000.000000000000000 ) ;
#5088 = AXIS2_PLACEMENT_3D ( 'NONE', #12143, #1516, #9619 ) ;
#5089 = CARTESIAN_POINT ( 'NONE',  ( -1.828356344711647763, -3.563200125723189338, -8.617289688891624500E-15 ) ) ;
#5090 = ORIENTED_EDGE ( 'NONE', *, *, #1563, .T. ) ;
#5091 = AXIS2_PLACEMENT_3D ( 'NONE', #6090, #10956, #14373 ) ;
#5092 = CIRCLE ( 'NONE', #4140, 59.50000000000000000 ) ;
#5093 = DIRECTION ( 'NONE',  ( 1.000000000000000000, 0.000000000000000000, 0.000000000000000000 ) ) ;
#5094 = ORIENTED_EDGE ( 'NONE', *, *, #11313, .F. ) ;
#5095 = AXIS2_PLACEMENT_3D ( 'NONE', #14277, #7434, #7357 ) ;
#5096 = EDGE_CURVE ( 'NONE', #5511, #4396, #5671, .T. ) ;
#5097 = DIRECTION ( 'NONE',  ( 1.000000000000000000, 0.000000000000000000, -0.000000000000000000 ) ) ;
#5098 = CARTESIAN_POINT ( 'NONE',  ( -18.00000000000000355, 2.326828918379971365E-15, -45.50000000000000000 ) ) ;
#5099 = ORIENTED_EDGE ( 'NONE', *, *, #12668, .F. ) ;
#5100 = DIRECTION ( 'NONE',  ( 1.000000000000000000, 0.000000000000000000, 0.000000000000000000 ) ) ;
#5101 = AXIS2_PLACEMENT_3D ( 'NONE', #1987, #12320, #4202 ) ;
#5102 = CARTESIAN_POINT ( 'NONE',  ( -89.61631465359441506, 37.12029293941468211, -10.50000000000000000 ) ) ;
#5103 = ORIENTED_EDGE ( 'NONE', *, *, #43, .T. ) ;
#5104 = CARTESIAN_POINT ( 'NONE',  ( 45.89934640057532533, -26.49999999999987566, -10.50000000000000000 ) ) ;
#5105 = CIRCLE ( 'NONE', #11915, 53.55662432702593634 ) ;
#5106 = ORIENTED_EDGE ( 'NONE', *, *, #10791, .T. ) ;
#5107 = ADVANCED_FACE ( 'NONE', ( #7294 ), #6146, .T. ) ;
#5108 = AXIS2_PLACEMENT_3D ( 'NONE', #296, #6125, #10768 ) ;
#5109 = CARTESIAN_POINT ( 'NONE',  ( -2.449293598294708880E-16, 38.00000000000000000, -28.00000000000000000 ) ) ;
#5110 = CARTESIAN_POINT ( 'NONE',  ( -13.58799986788203640, 50.71110588017617005, -10.50000000000000000 ) ) ;
#5111 = CARTESIAN_POINT ( 'NONE',  ( -31.47058823529411242, 102.2673069760056421, -11.33188329630078606 ) ) ;
#5112 = CARTESIAN_POINT ( 'NONE',  ( 51.45950017607693638, -4.121772567811421872, 8.000000000000000000 ) ) ;
#5113 = CIRCLE ( 'NONE', #15, 4.000000000000000000 ) ;
#5114 = DIRECTION ( 'NONE',  ( 0.000000000000000000, 0.000000000000000000, -1.000000000000000000 ) ) ;
#5115 = CIRCLE ( 'NONE', #13596, 3.000000000000002665 ) ;
#5116 = ORIENTED_EDGE ( 'NONE', *, *, #12309, .T. ) ;
#5117 = ADVANCED_BREP_SHAPE_REPRESENTATION ( '', ( #9171, #5108 ), #2434 ) ;
#5118 = DIRECTION ( 'NONE',  ( 0.9557692240748190127, -0.2941176470588235392, 6.631981242474902501E-16 ) ) ;
#5119 = CIRCLE ( 'NONE', #8268, 56.99999999999999289 ) ;
#5120 = FACE_OUTER_BOUND ( 'NONE', #5751, .T. ) ;
#5121 = AXIS2_PLACEMENT_3D ( 'NONE', #12359, #6493, #13425 ) ;
#5122 = DIRECTION ( 'NONE',  ( 0.000000000000000000, 0.000000000000000000, 1.000000000000000000 ) ) ;
#5123 = PRODUCT ( 'socket head cap screw_iso_ISO 4762 M5 x 50 - 22N', 'socket head cap screw_iso_ISO 4762 M5 x 50 - 22N', '', ( #5282 ) ) ;
#5124 = ORIENTED_EDGE ( 'NONE', *, *, #14735, .F. ) ;
#5125 = CARTESIAN_POINT ( 'NONE',  ( -12.94095225512574920, 48.29629131445349799, 8.000000000000000000 ) ) ;
#5126 = ORIENTED_EDGE ( 'NONE', *, *, #2182, .T. ) ;
#5127 = DIRECTION ( 'NONE',  ( 0.000000000000000000, 0.000000000000000000, -1.000000000000000000 ) ) ;
#5128 = CARTESIAN_POINT ( 'NONE',  ( -8.635299310232698033, 74.50321615228340022, 19.90320263233616771 ) ) ;
#5129 = ORIENTED_EDGE ( 'NONE', *, *, #1477, .T. ) ;
#5130 = CARTESIAN_POINT ( 'NONE',  ( -41.59008834022669987, -32.46576781417940794, -13.00000000000000178 ) ) ;
#5131 = CIRCLE ( 'NONE', #14839, 60.50000000000000000 ) ;
#5132 = DIRECTION ( 'NONE',  ( 0.000000000000000000, 0.000000000000000000, -1.000000000000000000 ) ) ;
#5133 = DIRECTION ( 'NONE',  ( 0.000000000000000000, 0.000000000000000000, 1.000000000000000000 ) ) ;
#5134 = CARTESIAN_POINT ( 'NONE',  ( -30.33578517098776217, 96.33676874097989185, -13.50363573142180584 ) ) ;
#5135 = VERTEX_POINT ( 'NONE', #6080 ) ;
#5136 = EDGE_CURVE ( 'NONE', #11371, #7026, #3672, .T. ) ;
#5137 = CARTESIAN_POINT ( 'NONE',  ( 52.54657765281197612, -6.917888187662545540, 8.000000000000000000 ) ) ;
#5139 = EDGE_CURVE ( 'NONE', #11359, #6102, #468, .T. ) ;
#5138 = DIRECTION ( 'NONE',  ( 0.000000000000000000, 0.000000000000000000, 1.000000000000000000 ) ) ;
#5140 = CIRCLE ( 'NONE', #12654, 10.00000000000000355 ) ;
#5141 = FACE_OUTER_BOUND ( 'NONE', #10746, .T. ) ;
#5142 = ORIENTED_EDGE ( 'NONE', *, *, #9016, .F. ) ;
#5143 = AXIS2_PLACEMENT_3D ( 'NONE', #10158, #10321, #5684 ) ;
#5144 = VERTEX_POINT ( 'NONE', #400 ) ;
#5145 = CARTESIAN_POINT ( 'NONE',  ( -92.38795325112907619, -38.26834323650805914, 8.000000000000000000 ) ) ;
#5146 = ORIENTED_EDGE ( 'NONE', *, *, #5083, .T. ) ;
#5147 = B_SPLINE_CURVE_WITH_KNOTS ( 'NONE', 3,
 ( #6057, #306, #3650, #8272, #5986, #8564 ),
 .UNSPECIFIED., .F., .F.,
 ( 4, 2, 4 ),
 ( 0.000000000000000000, 0.0002095117440864791795, 0.0004190234881729583589 ),
 .UNSPECIFIED. ) ;
#5148 = CARTESIAN_POINT ( 'NONE',  ( -25.00000000000000000, 81.24038404635962252, -26.00000000000000000 ) ) ;
#5149 = AXIS2_PLACEMENT_3D ( 'NONE', #9294, #10365, #12868 ) ;
#5150 = CARTESIAN_POINT ( 'NONE',  ( 4.141042297810614059, -2.227970268150435640, -3.687027686973625151 ) ) ;
#5151 = EDGE_CURVE ( 'NONE', #4677, #1124, #3250, .T. ) ;
#5152 = EDGE_LOOP ( 'NONE', ( #3000, #966, #13481, #3902 ) ) ;
#5153 = ORIENTED_EDGE ( 'NONE', *, *, #13690, .T. ) ;
#5154 = CARTESIAN_POINT ( 'NONE',  ( 26.00011991137315803, 45.91029614918951296, -10.50000000000000000 ) ) ;
#5155 = DIRECTION ( 'NONE',  ( 1.000000000000000000, 0.000000000000000000, -0.000000000000000000 ) ) ;
#5156 = ORIENTED_EDGE ( 'NONE', *, *, #7393, .F. ) ;
#5157 = EDGE_CURVE ( 'NONE', #5547, #10917, #7699, .T. ) ;
#5158 = CYLINDRICAL_SURFACE ( 'NONE', #5088, 60.50000000000000000 ) ;
#5159 = VERTEX_POINT ( 'NONE', #9418 ) ;
#5160 = AXIS2_PLACEMENT_3D ( 'NONE', #7983, #13776, #9050 ) ;
#5161 = ORIENTED_EDGE ( 'NONE', *, *, #485, .F. ) ;
#5162 = FACE_OUTER_BOUND ( 'NONE', #9531, .T. ) ;
#5163 = CIRCLE ( 'NONE', #13655, 3.000000000000002665 ) ;
#5164 = DIRECTION ( 'NONE',  ( -0.000000000000000000, -0.000000000000000000, 1.000000000000000000 ) ) ;
#5165 = DIRECTION ( 'NONE',  ( 0.000000000000000000, 0.000000000000000000, -1.000000000000000000 ) ) ;
#5166 = CARTESIAN_POINT ( 'NONE',  ( -32.26435573746199736, 42.04772703543562073, -13.00000000000000178 ) ) ;
#5167 = CARTESIAN_POINT ( 'NONE',  ( -1.312671235360383548, -3.860931062424225235, -0.05923475698271134932 ) ) ;
#5168 = CIRCLE ( 'NONE', #6618, 2.649999999999985700 ) ;
#5169 = VERTEX_POINT ( 'NONE', #7146 ) ;
#5170 = CARTESIAN_POINT ( 'NONE',  ( 0.000000000000000000, 0.000000000000000000, 8.000000000000000000 ) ) ;
#5171 = DIRECTION ( 'NONE',  ( 1.000000000000000000, 0.000000000000000000, 0.000000000000000000 ) ) ;
#5172 = CARTESIAN_POINT ( 'NONE',  ( -51.19406879332065330, -13.71740939043347041, -10.50000000000000000 ) ) ;
#5173 = ADVANCED_FACE ( 'NONE', ( #6157 ), #14145, .T. ) ;
#5174 = AXIS2_PLACEMENT_3D ( 'NONE', #12943, #1405, #6092 ) ;
#5175 = EDGE_CURVE ( 'NONE', #4338, #7227, #840, .T. ) ;
#5176 = ORIENTED_EDGE ( 'NONE', *, *, #2023, .T. ) ;
#5177 = CARTESIAN_POINT ( 'NONE',  ( -36.14014761921588104, 11.74264578624790190, 14.49999999999999822 ) ) ;
#5178 = ORIENTED_EDGE ( 'NONE', *, *, #595, .T. ) ;
#5179 = CARTESIAN_POINT ( 'NONE',  ( -37.12029293941441210, -89.61631465359452875, -10.50000000000000000 ) ) ;
#5180 = VECTOR ( 'NONE', #11483, 1000.000000000000000 ) ;
#5181 = ORIENTED_EDGE ( 'NONE', *, *, #14663, .T. ) ;
#5182 = DIRECTION ( 'NONE',  ( 0.000000000000000000, 0.000000000000000000, 1.000000000000000000 ) ) ;
#5183 = ORIENTED_EDGE ( 'NONE', *, *, #13412, .F. ) ;
#5184 = LINE ( 'NONE', #4055, #5692 ) ;
#5185 = DIRECTION ( 'NONE',  ( 0.000000000000000000, 0.000000000000000000, 1.000000000000000000 ) ) ;
#5186 = FACE_OUTER_BOUND ( 'NONE', #13858, .T. ) ;
#5187 = AXIS2_PLACEMENT_3D ( 'NONE', #174, #3897, #1619 ) ;
#5188 = EDGE_CURVE ( 'NONE', #7196, #1809, #1397, .T. ) ;
#5189 = CIRCLE ( 'NONE', #11514, 100.0000000000000000 ) ;
#5190 = DIRECTION ( 'NONE',  ( -0.000000000000000000, -0.000000000000000000, -1.000000000000000000 ) ) ;
#5191 = DIRECTION ( 'NONE',  ( 0.000000000000000000, 0.000000000000000000, 1.000000000000000000 ) ) ;
#5192 = DIRECTION ( 'NONE',  ( -1.000000000000000000, 0.000000000000000000, 0.000000000000000000 ) ) ;
#5193 = EDGE_LOOP ( 'NONE', ( #7674, #1503, #1860, #3859 ) ) ;
#5194 = ORIENTED_EDGE ( 'NONE', *, *, #2824, .T. ) ;
#5195 = DIRECTION ( 'NONE',  ( 0.000000000000000000, 0.000000000000000000, 1.000000000000000000 ) ) ;
#5196 = CARTESIAN_POINT ( 'NONE',  ( -18.00000000000000355, 2.204364238465235822E-15, -45.50000000000000000 ) ) ;
#5197 = EDGE_CURVE ( 'NONE', #12354, #10213, #8574, .T. ) ;
#5198 = CONICAL_SURFACE ( 'NONE', #7119, 2.500000000000000888, 0.9599310885968785900 ) ;
#5199 = DIRECTION ( 'NONE',  ( -1.000000000000000000, -5.306212985340821979E-15, 0.000000000000000000 ) ) ;
#5200 = VECTOR ( 'NONE', #3558, 1000.000000000000000 ) ;
#5201 = ORIENTED_EDGE ( 'NONE', *, *, #11920, .T. ) ;
#5202 = ORIENTED_EDGE ( 'NONE', *, *, #6567, .F. ) ;
#5203 = VERTEX_POINT ( 'NONE', #13080 ) ;
#5204 = DIRECTION ( 'NONE',  ( -1.000000000000000000, 0.000000000000000000, 0.000000000000000000 ) ) ;
#5205 = LINE ( 'NONE', #8259, #10473 ) ;
#5206 = AXIS2_PLACEMENT_3D ( 'NONE', #13120, #14765, #6196 ) ;
#5207 = CARTESIAN_POINT ( 'NONE',  ( 12.39897948556635399, 61.76783392443435616, -16.00000000000000000 ) ) ;
#5208 = CARTESIAN_POINT ( 'NONE',  ( 2.500000000000002220, 2.357898499370430834, -6.938893903907228378E-15 ) ) ;
#5209 = CARTESIAN_POINT ( 'NONE',  ( -36.14014761921588104, 11.74264578624790190, 19.50000000000000000 ) ) ;
#5210 = CARTESIAN_POINT ( 'NONE',  ( -30.68146655995339245, 96.22723358344983069, -14.04702900388066311 ) ) ;
#5211 = CIRCLE ( 'NONE', #7132, 3.000000000000002665 ) ;
#5212 = AXIS2_PLACEMENT_3D ( 'NONE', #7529, #12044, #4980 ) ;
#5213 = CIRCLE ( 'NONE', #8361, 50.00000000000000000 ) ;
#5214 = ORIENTED_EDGE ( 'NONE', *, *, #8567, .T. ) ;
#5215 = DIRECTION ( 'NONE',  ( -1.000000000000000000, 0.000000000000000000, 0.000000000000000000 ) ) ;
#5216 = DIRECTION ( 'NONE',  ( -1.000000000000000000, 0.000000000000000000, 0.000000000000000000 ) ) ;
#5217 = FACE_OUTER_BOUND ( 'NONE', #2419, .T. ) ;
#5218 = ORIENTED_EDGE ( 'NONE', *, *, #5549, .T. ) ;
#5219 = AXIS2_PLACEMENT_3D ( 'NONE', #1539, #7143, #11800 ) ;
#5220 = ORIENTED_EDGE ( 'NONE', *, *, #7408, .T. ) ;
#5221 = CARTESIAN_POINT ( 'NONE',  ( 9.706953719245472456, 57.06275842387054098, -8.000000000000000000 ) ) ;
#5222 = AXIS2_PLACEMENT_3D ( 'NONE', #8153, #8300, #10580 ) ;
#5223 = AXIS2_PLACEMENT_3D ( 'NONE', #4708, #6893, #5978 ) ;
#5224 = ORIENTED_EDGE ( 'NONE', *, *, #9173, .F. ) ;
#5225 = EDGE_CURVE ( 'NONE', #7077, #7439, #2043, .T. ) ;
#5226 = LINE ( 'NONE', #8697, #13687 ) ;
#5227 = CARTESIAN_POINT ( 'NONE',  ( 36.14014761921570340, 11.74264578624841171, -28.00000000000000000 ) ) ;
#5228 = ORIENTED_EDGE ( 'NONE', *, *, #8091, .F. ) ;
#5229 = CIRCLE ( 'NONE', #3547, 44.89637028918153305 ) ;
#5230 = CARTESIAN_POINT ( 'NONE',  ( -87.95718916809170196, 34.62083247296289557, -13.00000000000000178 ) ) ;
#5231 = CARTESIAN_POINT ( 'NONE',  ( 0.000000000000000000, 0.000000000000000000, 8.000000000000000000 ) ) ;
#5232 = EDGE_LOOP ( 'NONE', ( #9315, #10423, #6868, #8084, #329 ) ) ;
#5233 = DIRECTION ( 'NONE',  ( -0.000000000000000000, -0.000000000000000000, 1.000000000000000000 ) ) ;
#5234 = ORIENTED_EDGE ( 'NONE', *, *, #1131, .T. ) ;
#5235 = VERTEX_POINT ( 'NONE', #2676 ) ;
#5237 = ORIENTED_EDGE ( 'NONE', *, *, #1854, .F. ) ;
#5236 = APPLICATION_CONTEXT ( 'automotive_design' ) ;
#5238 = DIRECTION ( 'NONE',  ( -0.000000000000000000, -0.000000000000000000, 1.000000000000000000 ) ) ;
#5239 = AXIS2_PLACEMENT_3D ( 'NONE', #8319, #12661, #1192 ) ;
#5240 = EDGE_CURVE ( 'NONE', #1468, #8993, #1310, .T. ) ;
#5241 = ADVANCED_FACE ( 'NONE', ( #8513 ), #13157, .T. ) ;
#5242 = EDGE_CURVE ( 'NONE', #7769, #14730, #3748, .T. ) ;
#5243 = DIRECTION ( 'NONE',  ( 0.000000000000000000, 0.000000000000000000, 1.000000000000000000 ) ) ;
#5244 = DIRECTION ( 'NONE',  ( -0.000000000000000000, -0.000000000000000000, -1.000000000000000000 ) ) ;
#5245 = FACE_OUTER_BOUND ( 'NONE', #8518, .T. ) ;
#5246 = LINE ( 'NONE', #14739, #487 ) ;
#5247 = DIRECTION ( 'NONE',  ( 0.000000000000000000, 0.000000000000000000, 1.000000000000000000 ) ) ;
#5248 = VERTEX_POINT ( 'NONE', #8371 ) ;
#5249 = VECTOR ( 'NONE', #3911, 1000.000000000000114 ) ;
#5250 = DIRECTION ( 'NONE',  ( 0.000000000000000000, 0.000000000000000000, 1.000000000000000000 ) ) ;
#5251 = CARTESIAN_POINT ( 'NONE',  ( 17.27884612037405887, 39.14960378788569528, 11.00000000000000000 ) ) ;
#5252 = CARTESIAN_POINT ( 'NONE',  ( -18.52941176470586981, 60.21346111671361001, -26.00000000000000000 ) ) ;
#5253 = FACE_OUTER_BOUND ( 'NONE', #14034, .T. ) ;
#5254 = ORIENTED_EDGE ( 'NONE', *, *, #8070, .T. ) ;
#5255 = CARTESIAN_POINT ( 'NONE',  ( 0.000000000000000000, 0.000000000000000000, 0.000000000000000000 ) ) ;
#5256 = CARTESIAN_POINT ( 'NONE',  ( 3.999999999999995559, 0.7924765000094657896, -0.05906175389889570942 ) ) ;
#5257 = ORIENTED_EDGE ( 'NONE', *, *, #4353, .T. ) ;
#5258 = AXIS2_PLACEMENT_3D ( 'NONE', #6758, #11583, #11644 ) ;
#5259 = FACE_OUTER_BOUND ( 'NONE', #7509, .T. ) ;
#5260 = VERTEX_POINT ( 'NONE', #13237 ) ;
#5261 = PLANE ( 'NONE',  #2785 ) ;
#5262 = DIRECTION ( 'NONE',  ( 1.000000000000000000, 0.000000000000000000, 0.000000000000000000 ) ) ;
#5263 = CARTESIAN_POINT ( 'NONE',  ( 0.000000000000000000, 4.618802153517009401, -3.433295621305381573 ) ) ;
#5264 = CARTESIAN_POINT ( 'NONE',  ( -35.50766591049261223, 100.5715065882092745, -15.96896126722779208 ) ) ;
#5265 = ADVANCED_FACE ( 'NONE', ( #2831 ), #7444, .T. ) ;
#5266 = DIRECTION ( 'NONE',  ( 0.000000000000000000, 0.000000000000000000, -1.000000000000000000 ) ) ;
#5267 = CARTESIAN_POINT ( 'NONE',  ( -12.05137958362237960, 94.23255994477487718, 17.08976535968791310 ) ) ;
#5268 = EDGE_CURVE ( 'NONE', #6561, #5962, #9872, .T. ) ;
#5269 = VERTEX_POINT ( 'NONE', #3126 ) ;
#5270 = CARTESIAN_POINT ( 'NONE',  ( -2.775557561562891351E-14, -4.618802153517009401, -0.5000000000000004441 ) ) ;
#5271 = PLANE ( 'NONE',  #4494 ) ;
#5272 = CARTESIAN_POINT ( 'NONE',  ( -34.12029293941441210, -89.61631465359452875, 8.000000000000000000 ) ) ;
#5273 = EDGE_LOOP ( 'NONE', ( #10271, #11563, #6555, #10631, #8283 ) ) ;
#5274 = CARTESIAN_POINT ( 'NONE',  ( -4.235886605889385592, -2.417314728048545192, -3.751161874094021798 ) ) ;
#5275 = VERTEX_POINT ( 'NONE', #1838 ) ;
#5276 = CARTESIAN_POINT ( 'NONE',  ( 0.000000000000000000, 0.000000000000000000, -25.50000000000000355 ) ) ;
#5277 = DIRECTION ( 'NONE',  ( -1.000000000000000000, 0.000000000000000000, 0.000000000000000000 ) ) ;
#5278 = ADVANCED_FACE ( 'NONE', ( #14600 ), #8811, .F. ) ;
#5279 = DIRECTION ( 'NONE',  ( 0.000000000000000000, 0.000000000000000000, 1.000000000000000000 ) ) ;
#5280 = EDGE_CURVE ( 'NONE', #9491, #12422, #11741, .T. ) ;
#5281 = CARTESIAN_POINT ( 'NONE',  ( 27.94117647058824616, 90.79807628710781842, -13.50000000000000178 ) ) ;
#5282 = PRODUCT_CONTEXT ( 'NONE', #1442, 'mechanical' ) ;
#5283 = ORIENTED_EDGE ( 'NONE', *, *, #5369, .T. ) ;
#5284 = ORIENTED_EDGE ( 'NONE', *, *, #10369, .T. ) ;
#5285 = DIRECTION ( 'NONE',  ( 0.000000000000000000, 0.000000000000000000, -1.000000000000000000 ) ) ;
#5286 = DIRECTION ( 'NONE',  ( 1.000000000000000000, 0.000000000000000000, 0.000000000000000000 ) ) ;
#5287 = DIRECTION ( 'NONE',  ( 0.000000000000000000, 0.000000000000000000, 1.000000000000000000 ) ) ;
#5288 = ORIENTED_EDGE ( 'NONE', *, *, #8157, .F. ) ;
#5289 = EDGE_CURVE ( 'NONE', #479, #879, #13433, .T. ) ;
#5290 = VECTOR ( 'NONE', #7506, 1000.000000000000000 ) ;
#5291 = EDGE_LOOP ( 'NONE', ( #7391, #5930, #13969, #702, #12951, #2909, #8314, #14243, #6271, #5014, #13209, #12465, #4934, #10001, #8883, #13028, #1373, #4344, #5465, #4309 ) ) ;
#5292 = EDGE_LOOP ( 'NONE', ( #10833, #12967, #4790, #1507, #7139 ) ) ;
#5293 = FACE_OUTER_BOUND ( 'NONE', #771, .T. ) ;
#5294 = ADVANCED_FACE ( 'NONE', ( #5323, #4346, #6370, #12390, #4200, #12246, #11177 ), #8732, .T. ) ;
#5295 = DIRECTION ( 'NONE',  ( 0.000000000000000000, 0.000000000000000000, 1.000000000000000000 ) ) ;
#5296 = CARTESIAN_POINT ( 'NONE',  ( -2.649999999999989697, 38.00000000000000000, -25.50000000000000355 ) ) ;
#5297 = ORIENTED_EDGE ( 'NONE', *, *, #5157, .T. ) ;
#5298 = DIRECTION ( 'NONE',  ( -1.000000000000000000, 0.000000000000000000, -0.000000000000000000 ) ) ;
#5299 = CARTESIAN_POINT ( 'NONE',  ( -57.06275842387042729, 9.706953719246069312, -10.50000000000000000 ) ) ;
#5300 = ORIENTED_EDGE ( 'NONE', *, *, #7634, .T. ) ;
#5301 = CARTESIAN_POINT ( 'NONE',  ( 71.53347797788771345, 69.16568774265620334, -8.000000000000000000 ) ) ;
#5302 = ORIENTED_EDGE ( 'NONE', *, *, #12983, .F. ) ;
#5303 = ORIENTED_EDGE ( 'NONE', *, *, #7034, .T. ) ;
#5304 = ORIENTED_EDGE ( 'NONE', *, *, #10895, .T. ) ;
#5305 = DIRECTION ( 'NONE',  ( -1.000000000000000000, 0.000000000000000000, 0.000000000000000000 ) ) ;
#5306 = CARTESIAN_POINT ( 'NONE',  ( 0.000000000000000000, 0.000000000000000000, -8.000000000000000000 ) ) ;
#5307 = CIRCLE ( 'NONE', #13808, 59.50000000000000000 ) ;
#5308 = DIRECTION ( 'NONE',  ( 1.000000000000000000, 0.000000000000000000, 0.000000000000000000 ) ) ;
#5309 = CARTESIAN_POINT ( 'NONE',  ( 0.000000000000000000, 0.000000000000000000, -10.50000000000000000 ) ) ;
#5310 = DIRECTION ( 'NONE',  ( 0.000000000000000000, 0.000000000000000000, 1.000000000000000000 ) ) ;
#5311 = ORIENTED_EDGE ( 'NONE', *, *, #1728, .T. ) ;
#5312 = EDGE_CURVE ( 'NONE', #8196, #12042, #9053, .T. ) ;
#5313 = AXIS2_PLACEMENT_3D ( 'NONE', #5209, #3926, #12278 ) ;
#5314 = CYLINDRICAL_SURFACE ( 'NONE', #9990, 2.649999999999992806 ) ;
#5315 = EDGE_CURVE ( 'NONE', #9534, #13716, #3007, .T. ) ;
#5316 = EDGE_CURVE ( 'NONE', #4479, #6344, #342, .T. ) ;
#5317 = CARTESIAN_POINT ( 'NONE',  ( -97.00000000000000000, 1.015776140243522349E-12, -13.00000000000000178 ) ) ;
#5318 = VECTOR ( 'NONE', #3640, 1000.000000000000000 ) ;
#5319 = CARTESIAN_POINT ( 'NONE',  ( 4.211140560182194292, 2.431303136016534250, -3.745885042887433958 ) ) ;
#5320 = VERTEX_POINT ( 'NONE', #7675 ) ;
#5321 = CARTESIAN_POINT ( 'NONE',  ( 33.83210567914650824, 95.16559600367021687, -15.96768719852781615 ) ) ;
#5322 = VERTEX_POINT ( 'NONE', #3204 ) ;
#5323 = FACE_BOUND ( 'NONE', #2664, .T. ) ;
#5324 = ORIENTED_EDGE ( 'NONE', *, *, #11600, .F. ) ;
#5325 = CARTESIAN_POINT ( 'NONE',  ( -14.07862063237857342, 50.84834283437004387, -10.50000000000000000 ) ) ;
#5326 = ADVANCED_FACE ( 'NONE', ( #7821 ), #13200, .T. ) ;
#5327 = VERTEX_POINT ( 'NONE', #1903 ) ;
#5328 = CIRCLE ( 'NONE', #9443, 55.00000000000000000 ) ;
#5329 = CARTESIAN_POINT ( 'NONE',  ( 0.000000000000000000, 0.000000000000000000, -31.00000000000000000 ) ) ;
#5331 = CARTESIAN_POINT ( 'NONE',  ( 0.000000000000000000, 0.000000000000000000, 10.50000000000000000 ) ) ;
#5330 = AXIS2_PLACEMENT_3D ( 'NONE', #15000, #5725, #1404 ) ;
#5332 = CARTESIAN_POINT ( 'NONE',  ( 26.99988008862626643, 45.88839665196127271, -13.00000000000000178 ) ) ;
#5333 = CIRCLE ( 'NONE', #4615, 2.649999999999985700 ) ;
#5334 = CARTESIAN_POINT ( 'NONE',  ( -38.79014761921587251, 11.74264578624790190, -25.50000000000000355 ) ) ;
#5336 = DIRECTION ( 'NONE',  ( -0.000000000000000000, -0.000000000000000000, 1.000000000000000000 ) ) ;
#5335 = AXIS2_PLACEMENT_3D ( 'NONE', #13439, #9860, #7499 ) ;
#5337 = EDGE_CURVE ( 'NONE', #11614, #1920, #6520, .T. ) ;
#5338 = CYLINDRICAL_SURFACE ( 'NONE', #13383, 20.00000000000000000 ) ;
#5339 = ORIENTED_EDGE ( 'NONE', *, *, #4866, .T. ) ;
#5340 = EDGE_CURVE ( 'NONE', #7513, #13653, #10027, .T. ) ;
#5341 = CYLINDRICAL_SURFACE ( 'NONE', #3805, 2.100000000000000089 ) ;
#5342 = FILL_AREA_STYLE ('',( #9180 ) ) ;
#5343 = DIRECTION ( 'NONE',  ( -0.000000000000000000, 1.000000000000000000, -0.000000000000000000 ) ) ;
#5344 = VECTOR ( 'NONE', #781, 1000.000000000000000 ) ;
#5345 = DIRECTION ( 'NONE',  ( 0.000000000000000000, 0.000000000000000000, -1.000000000000000000 ) ) ;
#5346 = AXIS2_PLACEMENT_3D ( 'NONE', #12326, #2071, #1847 ) ;
#5347 = STYLED_ITEM ( 'NONE', ( #6720 ), #2938 ) ;
#5348 = ORIENTED_EDGE ( 'NONE', *, *, #14320, .T. ) ;
#5349 = FACE_OUTER_BOUND ( 'NONE', #4386, .T. ) ;
#5350 = ORIENTED_EDGE ( 'NONE', *, *, #2026, .T. ) ;
#5351 = FACE_OUTER_BOUND ( 'NONE', #4241, .T. ) ;
#5352 = DIRECTION ( 'NONE',  ( 0.000000000000000000, 0.000000000000000000, 1.000000000000000000 ) ) ;
#5353 = ORIENTED_EDGE ( 'NONE', *, *, #2586, .F. ) ;
#5354 = CIRCLE ( 'NONE', #1475, 3.000000000000002665 ) ;
#5355 = LINE ( 'NONE', #8838, #10179 ) ;
#5356 = DIRECTION ( 'NONE',  ( 0.000000000000000000, 0.000000000000000000, -1.000000000000000000 ) ) ;
#5357 =( NAMED_UNIT ( * ) PLANE_ANGLE_UNIT ( ) SI_UNIT ( $, .RADIAN. ) );
#5358 = VERTEX_POINT ( 'NONE', #4279 ) ;
#5359 = VECTOR ( 'NONE', #5992, 1000.000000000000000 ) ;
#5360 = EDGE_LOOP ( 'NONE', ( #14598, #9876, #8048, #13619, #13252, #6808, #10240, #11892, #1706, #14871 ) ) ;
#5361 = EDGE_LOOP ( 'NONE', ( #6682, #4333, #1666, #6470, #8363, #589 ) ) ;
#5362 = AXIS2_PLACEMENT_3D ( 'NONE', #1736, #8702, #13277 ) ;
#5363 = CARTESIAN_POINT ( 'NONE',  ( 52.36539807335608288, -6.451868917687384020, -13.00000000000000178 ) ) ;
#5364 = CARTESIAN_POINT ( 'NONE',  ( 11.10542050108867507, 94.34972528831985983, 18.51161449521946167 ) ) ;
#5365 = CARTESIAN_POINT ( 'NONE',  ( 51.49712671369393746, 14.70911110638358466, -10.50000000000000000 ) ) ;
#5366 = ORIENTED_EDGE ( 'NONE', *, *, #8976, .T. ) ;
#5367 = EDGE_CURVE ( 'NONE', #12937, #11617, #11006, .T. ) ;
#5368 = CIRCLE ( 'NONE', #5842, 50.00000000000000000 ) ;
#5369 = EDGE_CURVE ( 'NONE', #3649, #1924, #8093, .T. ) ;
#5370 = ORIENTED_EDGE ( 'NONE', *, *, #2126, .F. ) ;
#5371 = AXIS2_PLACEMENT_3D ( 'NONE', #2779, #4990, #14392 ) ;
#5372 = ORIENTED_EDGE ( 'NONE', *, *, #5791, .T. ) ;
#5373 = EDGE_CURVE ( 'NONE', #7535, #2855, #11880, .T. ) ;
#5374 = EDGE_CURVE ( 'NONE', #337, #3540, #2279, .T. ) ;
#5375 = CIRCLE ( 'NONE', #13867, 100.0000000000000000 ) ;
#5376 = DIRECTION ( 'NONE',  ( -0.5000000000000009992, 0.000000000000000000, 0.8660254037844380415 ) ) ;
#5377 = DIRECTION ( 'NONE',  ( 1.000000000000000000, 0.000000000000000000, 0.000000000000000000 ) ) ;
#5378 = PRESENTATION_STYLE_ASSIGNMENT (( #4017 ) ) ;
#5379 = DIRECTION ( 'NONE',  ( 0.000000000000000000, 0.000000000000000000, 1.000000000000000000 ) ) ;
#5380 = EDGE_CURVE ( 'NONE', #11838, #9110, #2212, .T. ) ;
#5381 = ORIENTED_EDGE ( 'NONE', *, *, #14406, .F. ) ;
#5383 = CIRCLE ( 'NONE', #12872, 3.000000000000004441 ) ;
#5382 = CARTESIAN_POINT ( 'NONE',  ( -6.917888187662729393, -52.54657765281195481, -13.00000000000000178 ) ) ;
#5384 = DIRECTION ( 'NONE',  ( -0.000000000000000000, -0.000000000000000000, 1.000000000000000000 ) ) ;
#5385 = VERTEX_POINT ( 'NONE', #12835 ) ;
#5386 = CARTESIAN_POINT ( 'NONE',  ( 44.89637028918153305, 5.498219616798048790E-15, 14.49999999999999822 ) ) ;
#5387 = AXIS2_PLACEMENT_3D ( 'NONE', #492, #7187, #146 ) ;
#5388 = ORIENTED_EDGE ( 'NONE', *, *, #5815, .T. ) ;
#5389 = EDGE_CURVE ( 'NONE', #10396, #4977, #98, .T. ) ;
#5390 = ORIENTED_EDGE ( 'NONE', *, *, #3061, .T. ) ;
#5391 = CARTESIAN_POINT ( 'NONE',  ( -29.70588235294118107, 96.53269163155674448, 10.99999999999999645 ) ) ;
#5392 = CARTESIAN_POINT ( 'NONE',  ( -92.55687898036933348, -36.52608637591544039, -13.00000000000000178 ) ) ;
#5393 = AXIS2_PLACEMENT_3D ( 'NONE', #4590, #9211, #409 ) ;
#5394 = PLANE ( 'NONE',  #3283 ) ;
#5395 = DIRECTION ( 'NONE',  ( -0.000000000000000000, -0.000000000000000000, -1.000000000000000000 ) ) ;
#5396 = DIRECTION ( 'NONE',  ( 0.000000000000000000, 0.000000000000000000, -1.000000000000000000 ) ) ;
#5397 = ORIENTED_EDGE ( 'NONE', *, *, #11477, .T. ) ;
#5398 = FACE_OUTER_BOUND ( 'NONE', #11693, .T. ) ;
#5399 = ORIENTED_EDGE ( 'NONE', *, *, #4416, .T. ) ;
#5400 = CIRCLE ( 'NONE', #11223, 2.055000000000000160 ) ;
#5401 = CYLINDRICAL_SURFACE ( 'NONE', #3728, 44.89637028918153305 ) ;
#5402 = PLANE ( 'NONE',  #7517 ) ;
#5403 = AXIS2_PLACEMENT_3D ( 'NONE', #1227, #11636, #9121 ) ;
#5404 = ORIENTED_EDGE ( 'NONE', *, *, #3413, .T. ) ;
#5405 = ORIENTED_EDGE ( 'NONE', *, *, #7396, .F. ) ;
#5406 = DIRECTION ( 'NONE',  ( 0.000000000000000000, 0.000000000000000000, -1.000000000000000000 ) ) ;
#5407 = ORIENTED_EDGE ( 'NONE', *, *, #13792, .F. ) ;
#5408 = CARTESIAN_POINT ( 'NONE',  ( -12.28299834225913223, 61.79111542428977799, 16.56818924177463614 ) ) ;
#5409 = EDGE_CURVE ( 'NONE', #7921, #14497, #10035, .T. ) ;
#5410 = EDGE_LOOP ( 'NONE', ( #13270, #128, #5350, #14325 ) ) ;
#5411 = AXIS2_PLACEMENT_3D ( 'NONE', #5565, #2231, #4740 ) ;
#5412 = CARTESIAN_POINT ( 'NONE',  ( -33.47282819776587814, 39.30189486418276346, -13.00000000000000178 ) ) ;
#5413 = CARTESIAN_POINT ( 'NONE',  ( -3.511755186886747371, 2.826662030176363860, -3.597382984111578974 ) ) ;
#5414 = EDGE_CURVE ( 'NONE', #11092, #12492, #11995, .T. ) ;
#5415 = CARTESIAN_POINT ( 'NONE',  ( 2.000000000000000444, 3.464101615137758383, -3.142992957459237235 ) ) ;
#5416 = EDGE_CURVE ( 'NONE', #9373, #12974, #6379, .T. ) ;
#5417 = AXIS2_PLACEMENT_3D ( 'NONE', #17, #7982, #12848 ) ;
#5418 = DIRECTION ( 'NONE',  ( 0.000000000000000000, 0.000000000000000000, 1.000000000000000000 ) ) ;
#5419 = CARTESIAN_POINT ( 'NONE',  ( -1.674280531759317014, 94.51066581171355097, -13.00000000000000178 ) ) ;
#5420 = DIRECTION ( 'NONE',  ( 0.000000000000000000, 0.000000000000000000, 1.000000000000000000 ) ) ;
#5421 = VERTEX_POINT ( 'NONE', #7970 ) ;
#5422 = LINE ( 'NONE', #6616, #8629 ) ;
#5423 = CARTESIAN_POINT ( 'NONE',  ( -89.12622059913283579, -37.21932736666236963, 10.49999999999999822 ) ) ;
#5424 = AXIS2_PLACEMENT_3D ( 'NONE', #12507, #11365, #7786 ) ;
#5425 = CARTESIAN_POINT ( 'NONE',  ( -37.53686968382306333, -89.89283556784496909, -13.00000000000000178 ) ) ;
#5426 = ORIENTED_EDGE ( 'NONE', *, *, #10637, .T. ) ;
#5427 = DIRECTION ( 'NONE',  ( 1.000000000000000000, 0.000000000000000000, 0.000000000000000000 ) ) ;
#5428 = AXIS2_PLACEMENT_3D ( 'NONE', #4527, #7848, #12499 ) ;
#5429 = ORIENTED_EDGE ( 'NONE', *, *, #4882, .F. ) ;
#5430 = LINE ( 'NONE', #8909, #10061 ) ;
#5431 = ADVANCED_FACE ( 'NONE', ( #12614 ), #6828, .F. ) ;
#5432 = FACE_OUTER_BOUND ( 'NONE', #6015, .T. ) ;
#5433 = ADVANCED_FACE ( 'NONE', ( #6681 ), #1320, .F. ) ;
#5434 = ORIENTED_EDGE ( 'NONE', *, *, #10092, .T. ) ;
#5435 = CARTESIAN_POINT ( 'NONE',  ( 89.89283556784508278, -37.53686968382275779, -10.50000000000000000 ) ) ;
#5436 = DIRECTION ( 'NONE',  ( 0.000000000000000000, 0.000000000000000000, -1.000000000000000000 ) ) ;
#5437 = ORIENTED_EDGE ( 'NONE', *, *, #2548, .F. ) ;
#5438 = ORIENTED_EDGE ( 'NONE', *, *, #14713, .T. ) ;
#5439 = APPLICATION_CONTEXT ( 'automotive_design' ) ;
#5440 = AXIS2_PLACEMENT_3D ( 'NONE', #10799, #10639, #14286 ) ;
#5441 = VECTOR ( 'NONE', #10145, 1000.000000000000000 ) ;
#5442 = LINE ( 'NONE', #8846, #10319 ) ;
#5443 = CARTESIAN_POINT ( 'NONE',  ( 25.00000000000000000, 81.24038404635960831, 31.00000000000000000 ) ) ;
#5444 = AXIS2_PLACEMENT_3D ( 'NONE', #2456, #7303, #7075 ) ;
#5445 = DIRECTION ( 'NONE',  ( 1.000000000000000000, 0.000000000000000000, 0.000000000000000000 ) ) ;
#5446 = VERTEX_POINT ( 'NONE', #8052 ) ;
#5447 = ORIENTED_EDGE ( 'NONE', *, *, #2605, .T. ) ;
#5448 = VERTEX_POINT ( 'NONE', #5701 ) ;
#5449 = AXIS2_PLACEMENT_3D ( 'NONE', #11573, #2134, #1007 ) ;
#5450 = CARTESIAN_POINT ( 'NONE',  ( 0.000000000000000000, 0.000000000000000000, -10.50000000000000000 ) ) ;
#5451 = TOROIDAL_SURFACE ( 'NONE', #3754, 4.000000000000000000, 0.2500000000000000000 ) ;
#5452 = DIRECTION ( 'NONE',  ( -0.000000000000000000, 0.000000000000000000, 1.000000000000000000 ) ) ;
#5453 = DIRECTION ( 'NONE',  ( 1.000000000000000000, 0.000000000000000000, -0.000000000000000000 ) ) ;
#5454 = DIRECTION ( 'NONE',  ( -1.000000000000000000, 0.000000000000000000, 0.000000000000000000 ) ) ;
#5455 = CARTESIAN_POINT ( 'NONE',  ( 52.54657765281197612, -6.917888187662545540, 10.49999999999999822 ) ) ;
#5456 = ADVANCED_FACE ( 'NONE', ( #9035 ), #7902, .F. ) ;
#5457 = ORIENTED_EDGE ( 'NONE', *, *, #9427, .T. ) ;
#5458 = CARTESIAN_POINT ( 'NONE',  ( 26.49999999999971578, 45.89934640057541060, -8.000000000000000000 ) ) ;
#5459 = ORIENTED_EDGE ( 'NONE', *, *, #10927, .T. ) ;
#5460 = AXIS2_PLACEMENT_3D ( 'NONE', #10905, #5566, #13197 ) ;
#5461 = EDGE_CURVE ( 'NONE', #2447, #7811, #12723, .T. ) ;
#5462 = CIRCLE ( 'NONE', #10547, 10.00000000000000178 ) ;
#5463 = ORIENTED_EDGE ( 'NONE', *, *, #4452, .T. ) ;
#5464 = CIRCLE ( 'NONE', #1583, 56.99999999999999289 ) ;
#5465 = ORIENTED_EDGE ( 'NONE', *, *, #9257, .F. ) ;
#5466 = CARTESIAN_POINT ( 'NONE',  ( 0.000000000000000000, 0.000000000000000000, -8.000000000000000000 ) ) ;
#5467 = ADVANCED_FACE ( 'NONE', ( #1157 ), #5767, .F. ) ;
#5468 = DIRECTION ( 'NONE',  ( 0.000000000000000000, 0.000000000000000000, -1.000000000000000000 ) ) ;
#5469 = AXIS2_PLACEMENT_3D ( 'NONE', #13832, #11487, #1085 ) ;
#5470 = CARTESIAN_POINT ( 'NONE',  ( 87.95718916809192933, -34.62083247296232713, -8.000000000000000000 ) ) ;
#5471 = CARTESIAN_POINT ( 'NONE',  ( -39.61975340586619865, -91.27544013909722764, -13.00000000000000178 ) ) ;
#5472 = VECTOR ( 'NONE', #2411, 1000.000000000000000 ) ;
#5473 = EDGE_CURVE ( 'NONE', #12128, #11525, #14902, .T. ) ;
#5474 = EDGE_CURVE ( 'NONE', #4441, #13877, #14271, .T. ) ;
#5475 = ORIENTED_EDGE ( 'NONE', *, *, #1474, .F. ) ;
#5476 = DIRECTION ( 'NONE',  ( 0.000000000000000000, -0.4999999999999995559, 0.8660254037844389297 ) ) ;
#5477 = VECTOR ( 'NONE', #4311, 1000.000000000000000 ) ;
#5478 = LINE ( 'NONE', #5970, #7089 ) ;
#5479 = DIRECTION ( 'NONE',  ( 1.000000000000000000, 0.000000000000000000, 0.000000000000000000 ) ) ;
#5480 = CIRCLE ( 'NONE', #4999, 63.00000000000000000 ) ;
#5481 = EDGE_LOOP ( 'NONE', ( #1436, #10869, #10187, #544 ) ) ;
#5482 = CARTESIAN_POINT ( 'NONE',  ( 33.23060097332286489, 95.37689352056796110, -15.83317473434553335 ) ) ;
#5483 = EDGE_CURVE ( 'NONE', #6523, #2474, #6161, .T. ) ;
#5484 = ORIENTED_EDGE ( 'NONE', *, *, #1125, .T. ) ;
#5485 = ORIENTED_EDGE ( 'NONE', *, *, #9890, .T. ) ;
#5486 = CARTESIAN_POINT ( 'NONE',  ( -12.39897948556635754, 61.76783392443436327, 16.00000000000000000 ) ) ;
#5487 = DIRECTION ( 'NONE',  ( 0.000000000000000000, 0.000000000000000000, 1.000000000000000000 ) ) ;
#5488 = CARTESIAN_POINT ( 'NONE',  ( -70.71067811865538033, -70.71067811865414399, -8.000000000000000000 ) ) ;
#5489 = PLANE ( 'NONE',  #12680 ) ;
#5490 = ORIENTED_EDGE ( 'NONE', *, *, #9090, .T. ) ;
#5491 = CYLINDRICAL_SURFACE ( 'NONE', #3864, 3.000000000000002665 ) ;
#5492 = CARTESIAN_POINT ( 'NONE',  ( -9.448652591187071792, 74.40292581525912397, -19.61336856585178623 ) ) ;
#5493 = DIRECTION ( 'NONE',  ( 0.000000000000000000, 0.000000000000000000, 1.000000000000000000 ) ) ;
#5494 = ORIENTED_EDGE ( 'NONE', *, *, #6776, .F. ) ;
#5495 = CARTESIAN_POINT ( 'NONE',  ( 14.07862063237891981, -50.84834283436993729, 10.49999999999999822 ) ) ;
#5496 = CARTESIAN_POINT ( 'NONE',  ( 11.08614924580848360, 94.35111528408442894, -18.49588680517285511 ) ) ;
#5497 = CARTESIAN_POINT ( 'NONE',  ( 2.649999999999993250, 38.00000000000000000, -28.00000000000000000 ) ) ;
#5498 = CIRCLE ( 'NONE', #13493, 0.5155456020628804703 ) ;
#5499 = VERTEX_POINT ( 'NONE', #5987 ) ;
#5500 = CARTESIAN_POINT ( 'NONE',  ( 0.000000000000000000, 0.000000000000000000, 10.50000000000000000 ) ) ;
#5501 = VERTEX_POINT ( 'NONE', #4946 ) ;
#5502 = B_SPLINE_CURVE_WITH_KNOTS ( 'NONE', 3,
 ( #4747, #9360, #7992, #12716, #1326, #5942, #12636, #13940 ),
 .UNSPECIFIED., .F., .F.,
 ( 4, 2, 2, 4 ),
 ( 2.465131517120937137E-07, 0.001183067374689842407, 0.001774477805458907686, 0.002365888236227972966 ),
 .UNSPECIFIED. ) ;
#5503 = DIRECTION ( 'NONE',  ( -1.000000000000000000, 0.000000000000000000, 0.000000000000000000 ) ) ;
#5504 = ORIENTED_EDGE ( 'NONE', *, *, #3620, .T. ) ;
#5505 = CARTESIAN_POINT ( 'NONE',  ( 0.000000000000000000, 0.000000000000000000, -8.000000000000000000 ) ) ;
#5506 = CARTESIAN_POINT ( 'NONE',  ( 68.58935777509523746, 68.58935777509499587, -8.000000000000000000 ) ) ;
#5507 = CARTESIAN_POINT ( 'NONE',  ( 9.714076971208447375, 106.5585699559772621, -19.49498877141799014 ) ) ;
#5508 = DIRECTION ( 'NONE',  ( -0.000000000000000000, -0.000000000000000000, 1.000000000000000000 ) ) ;
#5509 = VERTEX_POINT ( 'NONE', #3733 ) ;
#5510 = ORIENTED_EDGE ( 'NONE', *, *, #4353, .F. ) ;
#5511 = VERTEX_POINT ( 'NONE', #8493 ) ;
#5512 = EDGE_CURVE ( 'NONE', #8402, #4906, #4482, .T. ) ;
#5513 = DIRECTION ( 'NONE',  ( 0.000000000000000000, 0.000000000000000000, 1.000000000000000000 ) ) ;
#5514 = CARTESIAN_POINT ( 'NONE',  ( -33.48561063518626923, 47.21331623427104063, -8.000000000000000000 ) ) ;
#5515 = ADVANCED_FACE ( 'NONE', ( #4789 ), #6137, .F. ) ;
#5516 = DIRECTION ( 'NONE',  ( -0.2941176470588237613, -0.9557692240748189016, 0.000000000000000000 ) ) ;
#5517 = EDGE_CURVE ( 'NONE', #10139, #5169, #591, .T. ) ;
#5519 = VERTEX_POINT ( 'NONE', #8425 ) ;
#5518 = ADVANCED_FACE ( 'NONE', ( #11934 ), #13685, .T. ) ;
#5520 = VERTEX_POINT ( 'NONE', #2656 ) ;
#5521 = EDGE_LOOP ( 'NONE', ( #6783, #4119 ) ) ;
#5522 = CARTESIAN_POINT ( 'NONE',  ( -12.50000000000000000, 100.2235002382176248, 15.00000000000000000 ) ) ;
#5523 = B_SPLINE_CURVE_WITH_KNOTS ( 'NONE', 3,
 ( #10275, #4518, #4886, #9417, #3747 ),
 .UNSPECIFIED., .F., .F.,
 ( 4, 1, 4 ),
 ( 0.000000000000000000, 0.002309401076758506657, 0.004618802153517013315 ),
 .UNSPECIFIED. ) ;
#5524 = DIRECTION ( 'NONE',  ( -1.000000000000000000, 0.000000000000000000, 0.000000000000000000 ) ) ;
#5525 = PLANE ( 'NONE',  #13936 ) ;
#5526 = DIRECTION ( 'NONE',  ( 1.000000000000000000, 0.000000000000000000, 0.000000000000000000 ) ) ;
#5527 = CARTESIAN_POINT ( 'NONE',  ( 7.383907457638312799, 52.72775723226772726, 10.49999999999999822 ) ) ;
#5528 = CARTESIAN_POINT ( 'NONE',  ( -36.08010649850015028, 100.2464683348682684, 16.00000000000000000 ) ) ;
#5529 = ORIENTED_EDGE ( 'NONE', *, *, #744, .F. ) ;
#5530 = DIRECTION ( 'NONE',  ( -1.000000000000000000, 0.000000000000000000, 0.000000000000000000 ) ) ;
#5531 = AXIS2_PLACEMENT_3D ( 'NONE', #3852, #5060, #504 ) ;
#5532 = VERTEX_POINT ( 'NONE', #7048 ) ;
#5533 = ORIENTED_EDGE ( 'NONE', *, *, #13805, .F. ) ;
#5534 = CARTESIAN_POINT ( 'NONE',  ( 0.000000000000000000, 0.000000000000000000, -10.50000000000000000 ) ) ;
#5535 = EDGE_CURVE ( 'NONE', #452, #1155, #5925, .T. ) ;
#5536 = CARTESIAN_POINT ( 'NONE',  ( -12.39897948556635754, 100.2360479454198696, 16.00000000000000000 ) ) ;
#5537 = DIRECTION ( 'NONE',  ( -1.000000000000000000, 0.000000000000000000, 0.000000000000000000 ) ) ;
#5538 = FACE_OUTER_BOUND ( 'NONE', #9666, .T. ) ;
#5539 = CARTESIAN_POINT ( 'NONE',  ( -31.47058823529412663, 102.2673069760056563, -10.99999999999999645 ) ) ;
#5540 = DIRECTION ( 'NONE',  ( -0.000000000000000000, -0.000000000000000000, -1.000000000000000000 ) ) ;
#5541 = EDGE_LOOP ( 'NONE', ( #5854, #115, #7185, #1180, #11132, #6034, #8608, #13472, #9928, #9938, #2639, #8375 ) ) ;
#5542 = CIRCLE ( 'NONE', #9410, 52.50000000000000711 ) ;
#5543 = CARTESIAN_POINT ( 'NONE',  ( 49.00442420935993226, -30.80502811811213704, -13.00000000000000178 ) ) ;
#5544 = ORIENTED_EDGE ( 'NONE', *, *, #1309, .F. ) ;
#5545 = CARTESIAN_POINT ( 'NONE',  ( 47.21331623427115431, 33.48561063518610581, -13.00000000000000178 ) ) ;
#5546 = CARTESIAN_POINT ( 'NONE',  ( 0.000000000000000000, -4.862606272033110244, -3.745885042887441063 ) ) ;
#5547 = VERTEX_POINT ( 'NONE', #8274 ) ;
#5548 = DIRECTION ( 'NONE',  ( 1.000000000000000000, 0.000000000000000000, 0.000000000000000000 ) ) ;
#5549 = EDGE_CURVE ( 'NONE', #1483, #14940, #7616, .T. ) ;
#5550 = CARTESIAN_POINT ( 'NONE',  ( 92.61631465359468507, -37.12029293941410657, -13.00000000000000178 ) ) ;
#5551 = ADVANCED_FACE ( 'NONE', ( #14054 ), #7274, .F. ) ;
#5552 = EDGE_LOOP ( 'NONE', ( #6982, #347, #9488, #526, #13233, #11419 ) ) ;
#5553 = DIRECTION ( 'NONE',  ( -1.000000000000000000, 0.000000000000000000, 0.000000000000000000 ) ) ;
#5554 = LINE ( 'NONE', #5412, #1103 ) ;
#5555 = DIRECTION ( 'NONE',  ( 1.000000000000000000, 0.000000000000000000, 0.000000000000000000 ) ) ;
#5556 = DIRECTION ( 'NONE',  ( 1.000000000000000000, 0.000000000000000000, -0.000000000000000000 ) ) ;
#5557 = DIRECTION ( 'NONE',  ( 0.000000000000000000, 0.000000000000000000, -1.000000000000000000 ) ) ;
#5558 = CARTESIAN_POINT ( 'NONE',  ( 31.05588327715836527, -44.79355920668822932, 8.000000000000000000 ) ) ;
#5559 = EDGE_CURVE ( 'NONE', #12241, #6523, #10556, .T. ) ;
#5560 = CIRCLE ( 'NONE', #8457, 0.5000000000000022204 ) ;
#5561 = FILL_AREA_STYLE_COLOUR ( '', #6574 ) ;
#5562 = EDGE_LOOP ( 'NONE', ( #9322, #316, #679, #9636 ) ) ;
#5563 = CARTESIAN_POINT ( 'NONE',  ( 33.48561063518626923, -47.21331623427104063, -10.50000000000000000 ) ) ;
#5564 = FACE_OUTER_BOUND ( 'NONE', #7305, .T. ) ;
#5565 = CARTESIAN_POINT ( 'NONE',  ( 33.48561063518626923, -47.21331623427104063, 8.000000000000000000 ) ) ;
#5566 = DIRECTION ( 'NONE',  ( -0.000000000000000000, -0.000000000000000000, 1.000000000000000000 ) ) ;
#5567 = EDGE_CURVE ( 'NONE', #7442, #203, #12914, .T. ) ;
#5568 = ORIENTED_EDGE ( 'NONE', *, *, #7560, .T. ) ;
#5569 = CARTESIAN_POINT ( 'NONE',  ( 17.27884612037405887, 39.14960378788569528, 16.00000000000000000 ) ) ;
#5570 = ORIENTED_EDGE ( 'NONE', *, *, #8166, .T. ) ;
#5571 = DIRECTION ( 'NONE',  ( 0.000000000000000000, 0.000000000000000000, -1.000000000000000000 ) ) ;
#5572 = DIRECTION ( 'NONE',  ( -0.8660254037844377084, -0.5000000000000015543, 0.000000000000000000 ) ) ;
#5573 = LINE ( 'NONE', #956, #4379 ) ;
#5574 = LINE ( 'NONE', #9062, #6866 ) ;
#5575 = ORIENTED_EDGE ( 'NONE', *, *, #2233, .F. ) ;
#5576 = ORIENTED_EDGE ( 'NONE', *, *, #6567, .T. ) ;
#5577 = ORIENTED_EDGE ( 'NONE', *, *, #6609, .T. ) ;
#5578 = ORIENTED_EDGE ( 'NONE', *, *, #10051, .T. ) ;
#5579 = CIRCLE ( 'NONE', #9715, 0.5000000000000004441 ) ;
#5580 = CARTESIAN_POINT ( 'NONE',  ( -22.33583958711380646, -30.74264578624812927, 14.49999999999999822 ) ) ;
#5581 = CYLINDRICAL_SURFACE ( 'NONE', #13686, 0.5000000000000073275 ) ;
#5582 = VECTOR ( 'NONE', #8801, 1000.000000000000000 ) ;
#5583 = DIRECTION ( 'NONE',  ( 0.000000000000000000, 0.000000000000000000, -1.000000000000000000 ) ) ;
#5584 = VERTEX_POINT ( 'NONE', #11853 ) ;
#5585 = VERTEX_POINT ( 'NONE', #1446 ) ;
#5586 = ORIENTED_EDGE ( 'NONE', *, *, #6664, .T. ) ;
#5587 = AXIS2_PLACEMENT_3D ( 'NONE', #13765, #8276, #14055 ) ;
#5588 = DIRECTION ( 'NONE',  ( 0.000000000000000000, 0.000000000000000000, 1.000000000000000000 ) ) ;
#5589 = AXIS2_PLACEMENT_3D ( 'NONE', #3587, #11635, #13767 ) ;
#5591 = CIRCLE ( 'NONE', #14082, 3.000000000000002665 ) ;
#5590 = CARTESIAN_POINT ( 'NONE',  ( 0.000000000000000000, 0.000000000000000000, -10.50000000000000000 ) ) ;
#5592 = DIRECTION ( 'NONE',  ( -0.000000000000000000, -0.000000000000000000, 1.000000000000000000 ) ) ;
#5593 = EDGE_CURVE ( 'NONE', #10072, #10139, #14419, .T. ) ;
#5594 = DIRECTION ( 'NONE',  ( -1.000000000000000000, 0.000000000000000000, 0.000000000000000000 ) ) ;
#5595 = EDGE_CURVE ( 'NONE', #9910, #14881, #4801, .T. ) ;
#5596 = DIRECTION ( 'NONE',  ( -0.000000000000000000, -0.000000000000000000, 1.000000000000000000 ) ) ;
#5597 = ORIENTED_EDGE ( 'NONE', *, *, #7115, .F. ) ;
#5598 = AXIS2_PLACEMENT_3D ( 'NONE', #5909, #12828, #2417 ) ;
#5599 = DIRECTION ( 'NONE',  ( 0.000000000000000000, 0.000000000000000000, -1.000000000000000000 ) ) ;
#5600 = CARTESIAN_POINT ( 'NONE',  ( 37.21932736666271779, -89.12622059913267947, 10.49999999999999822 ) ) ;
#5601 = CIRCLE ( 'NONE', #11435, 4.999999999999995559 ) ;
#5602 = ORIENTED_EDGE ( 'NONE', *, *, #4800, .T. ) ;
#5603 = AXIS2_PLACEMENT_3D ( 'NONE', #14646, #8929, #3177 ) ;
#5604 = VERTEX_POINT ( 'NONE', #11685 ) ;
#5605 = CARTESIAN_POINT ( 'NONE',  ( 41.65105036528968441, 31.95997502295806214, -10.50000000000000000 ) ) ;
#5606 = ADVANCED_FACE ( 'NONE', ( #8177 ), #3481, .T. ) ;
#5607 = CYLINDRICAL_SURFACE ( 'NONE', #1006, 60.50000000000000000 ) ;
#5608 = FACE_OUTER_BOUND ( 'NONE', #9729, .T. ) ;
#5609 = CIRCLE ( 'NONE', #4654, 59.49999999999999289 ) ;
#5610 = CARTESIAN_POINT ( 'NONE',  ( 42.04772703543530099, 32.26435573746242369, -13.00000000000000178 ) ) ;
#5611 = CARTESIAN_POINT ( 'NONE',  ( 12.50000000000000000, 106.2673515243510991, -15.00000000000000355 ) ) ;
#5612 = EDGE_CURVE ( 'NONE', #14961, #3015, #2052, .T. ) ;
#5613 = LINE ( 'NONE', #10249, #13329 ) ;
#5614 = AXIS2_PLACEMENT_3D ( 'NONE', #1106, #3675, #8151 ) ;
#5615 = ORIENTED_EDGE ( 'NONE', *, *, #6947, .T. ) ;
#5616 = PLANE ( 'NONE',  #14611 ) ;
#5617 = DIRECTION ( 'NONE',  ( 0.000000000000000000, 0.000000000000000000, 1.000000000000000000 ) ) ;
#5618 = CARTESIAN_POINT ( 'NONE',  ( -27.94117647058823550, 90.79807628710781842, 16.00000000000000000 ) ) ;
#5619 = CIRCLE ( 'NONE', #2712, 50.00000000000000000 ) ;
#5620 = EDGE_LOOP ( 'NONE', ( #7997, #6337, #3108, #2116, #7547, #10335 ) ) ;
#5621 = CARTESIAN_POINT ( 'NONE',  ( -5.384454397937118664, 6.594054843588581554E-16, -4.484454397937119197 ) ) ;
#5622 = EDGE_LOOP ( 'NONE', ( #3374, #2015, #8175, #319, #11691, #8953 ) ) ;
#5623 = DIRECTION ( 'NONE',  ( -0.000000000000000000, -0.000000000000000000, 1.000000000000000000 ) ) ;
#5624 = CIRCLE ( 'NONE', #13389, 50.00000000000000000 ) ;
#5625 = CARTESIAN_POINT ( 'NONE',  ( 89.61631465359491244, 37.12029293941346708, -13.00000000000000178 ) ) ;
#5626 = CARTESIAN_POINT ( 'NONE',  ( 68.58935777509523746, 68.58935777509499587, 10.49999999999999822 ) ) ;
#5627 = CARTESIAN_POINT ( 'NONE',  ( -87.95718916809170196, 34.62083247296289557, -8.000000000000000000 ) ) ;
#5628 = CARTESIAN_POINT ( 'NONE',  ( 71.53347797788772766, 69.16568774265620334, 8.000000000000000000 ) ) ;
#5629 = CARTESIAN_POINT ( 'NONE',  ( -12.86891638962156215, 56.43380494353993271, -13.00000000000000178 ) ) ;
#5630 = AXIS2_PLACEMENT_3D ( 'NONE', #10512, #2462, #9222 ) ;
#5631 = FACE_OUTER_BOUND ( 'NONE', #2627, .T. ) ;
#5632 = EDGE_CURVE ( 'NONE', #5663, #11040, #9318, .T. ) ;
#5633 =( NAMED_UNIT ( * ) PLANE_ANGLE_UNIT ( ) SI_UNIT ( $, .RADIAN. ) );
#5634 = EDGE_CURVE ( 'NONE', #7442, #1613, #6885, .T. ) ;
#5635 = VERTEX_POINT ( 'NONE', #1198 ) ;
#5636 = EDGE_CURVE ( 'NONE', #12743, #13570, #1093, .T. ) ;
#5637 = AXIS2_PLACEMENT_3D ( 'NONE', #10428, #10581, #10282 ) ;
#5638 = DIRECTION ( 'NONE',  ( -1.000000000000000000, 1.826024711554534406E-15, 0.000000000000000000 ) ) ;
#5639 = FACE_OUTER_BOUND ( 'NONE', #1411, .T. ) ;
#5640 = CARTESIAN_POINT ( 'NONE',  ( -46.24878538001294004, 27.00670028307212078, -10.50000000000000000 ) ) ;
#5641 = ORIENTED_EDGE ( 'NONE', *, *, #5016, .T. ) ;
#5642 = CARTESIAN_POINT ( 'NONE',  ( -12.39897948556635754, 61.76783392443436327, -16.00000000000000000 ) ) ;
#5643 = CIRCLE ( 'NONE', #12922, 3.000000000000002665 ) ;
#5644 = ORIENTED_EDGE ( 'NONE', *, *, #10561, .F. ) ;
#5645 = EDGE_CURVE ( 'NONE', #14119, #9063, #9548, .T. ) ;
#5646 = CARTESIAN_POINT ( 'NONE',  ( 2.449293598294700991E-16, -97.00000000000000000, -13.00000000000000178 ) ) ;
#5647 = ORIENTED_EDGE ( 'NONE', *, *, #4734, .F. ) ;
#5648 = AXIS2_PLACEMENT_3D ( 'NONE', #9570, #1459, #8580 ) ;
#5649 = DIRECTION ( 'NONE',  ( 0.000000000000000000, 0.000000000000000000, 1.000000000000000000 ) ) ;
#5650 = DIRECTION ( 'NONE',  ( 0.000000000000000000, 0.000000000000000000, -1.000000000000000000 ) ) ;
#5651 = CIRCLE ( 'NONE', #3229, 3.000000000000002665 ) ;
#5652 = DIRECTION ( 'NONE',  ( 0.000000000000000000, 0.000000000000000000, 1.000000000000000000 ) ) ;
#5653 = DIRECTION ( 'NONE',  ( -1.000000000000000000, 0.000000000000000000, 0.000000000000000000 ) ) ;
#5654 = VERTEX_POINT ( 'NONE', #8247 ) ;
#5655 = ADVANCED_FACE ( 'NONE', ( #11544 ), #11611, .F. ) ;
#5656 = VERTEX_POINT ( 'NONE', #1059 ) ;
#5657 = VERTEX_POINT ( 'NONE', #4621 ) ;
#5658 = CIRCLE ( 'NONE', #10748, 60.50000000000000000 ) ;
#5659 = ADVANCED_FACE ( 'NONE', ( #6802 ), #11754, .T. ) ;
#5660 = DIRECTION ( 'NONE',  ( 0.000000000000000000, 0.000000000000000000, 1.000000000000000000 ) ) ;
#5661 = CARTESIAN_POINT ( 'NONE',  ( -30.80502811811232888, -49.00442420935981147, -10.50000000000000000 ) ) ;
#5662 = CARTESIAN_POINT ( 'NONE',  ( -45.39934640057513349, 26.50000000000019540, -10.50000000000000000 ) ) ;
#5663 = VERTEX_POINT ( 'NONE', #7020 ) ;
#5664 = CIRCLE ( 'NONE', #14152, 63.00000000000000000 ) ;
#5665 = VERTEX_POINT ( 'NONE', #52 ) ;
#5666 = VERTEX_POINT ( 'NONE', #12888 ) ;
#5667 = FACE_OUTER_BOUND ( 'NONE', #4744, .T. ) ;
#5668 = CARTESIAN_POINT ( 'NONE',  ( 7.500000000000000000, 61.74746958378133144, 20.00000000000000000 ) ) ;
#5669 = DIRECTION ( 'NONE',  ( -1.000000000000000000, 0.000000000000000000, 0.000000000000000000 ) ) ;
#5670 = DIRECTION ( 'NONE',  ( -1.000000000000000000, 0.000000000000000000, 0.000000000000000000 ) ) ;
#5671 = CIRCLE ( 'NONE', #7361, 59.50000000000000711 ) ;
#5672 = AXIS2_PLACEMENT_3D ( 'NONE', #7451, #12102, #1694 ) ;
#5673 = EDGE_LOOP ( 'NONE', ( #1426, #4595, #1858, #1868 ) ) ;
#5674 = FACE_OUTER_BOUND ( 'NONE', #12953, .T. ) ;
#5675 = ORIENTED_EDGE ( 'NONE', *, *, #5877, .F. ) ;
#5676 = CARTESIAN_POINT ( 'NONE',  ( 0.000000000000000000, 0.000000000000000000, -45.50000000000000000 ) ) ;
#5677 = CARTESIAN_POINT ( 'NONE',  ( 0.000000000000000000, 0.000000000000000000, 8.000000000000000000 ) ) ;
#5678 = ORIENTED_EDGE ( 'NONE', *, *, #5374, .T. ) ;
#5679 = ORIENTED_EDGE ( 'NONE', *, *, #10951, .F. ) ;
#5680 = CARTESIAN_POINT ( 'NONE',  ( 92.38795325112852197, -38.26834323650938074, 8.000000000000000000 ) ) ;
#5681 = EDGE_CURVE ( 'NONE', #5962, #6738, #3751, .T. ) ;
#5682 = VECTOR ( 'NONE', #3875, 1000.000000000000000 ) ;
#5683 = CARTESIAN_POINT ( 'NONE',  ( -32.26435573746199736, 42.04772703543562073, 10.49999999999999822 ) ) ;
#5684 = DIRECTION ( 'NONE',  ( -1.000000000000000000, 0.000000000000000000, 0.000000000000000000 ) ) ;
#5685 = CARTESIAN_POINT ( 'NONE',  ( 72.70695371924547601, 57.06275842387054098, -8.000000000000000000 ) ) ;
#5686 = CARTESIAN_POINT ( 'NONE',  ( 2.500000000000002220, -1.178949249685208533, 2.042000000000002036 ) ) ;
#5687 = AXIS2_PLACEMENT_3D ( 'NONE', #9460, #14108, #11837 ) ;
#5688 = FACE_OUTER_BOUND ( 'NONE', #4045, .T. ) ;
#5689 = ORIENTED_EDGE ( 'NONE', *, *, #4180, .T. ) ;
#5690 = VECTOR ( 'NONE', #11830, 1000.000000000000000 ) ;
#5691 = LINE ( 'NONE', #10327, #8262 ) ;
#5692 = VECTOR ( 'NONE', #2898, 1000.000000000000000 ) ;
#5693 = CARTESIAN_POINT ( 'NONE',  ( 3.999999999999996447, -2.309401076758518911, -0.5000000000000004441 ) ) ;
#5694 = CARTESIAN_POINT ( 'NONE',  ( 0.000000000000000000, 0.000000000000000000, -10.50000000000000000 ) ) ;
#5695 = EDGE_CURVE ( 'NONE', #5665, #1689, #13212, .T. ) ;
#5696 = ORIENTED_EDGE ( 'NONE', *, *, #6502, .F. ) ;
#5697 = CYLINDRICAL_SURFACE ( 'NONE', #8596, 56.99999999999999289 ) ;
#5698 = EDGE_CURVE ( 'NONE', #13514, #14649, #10310, .T. ) ;
#5699 = EDGE_CURVE ( 'NONE', #7929, #10605, #14953, .T. ) ;
#5700 = AXIS2_PLACEMENT_3D ( 'NONE', #4943, #14125, #1598 ) ;
#5701 = CARTESIAN_POINT ( 'NONE',  ( -5.384454397937118664, 6.702023979852546576E-16, -5.000000000000000888 ) ) ;
#5702 = ORIENTED_EDGE ( 'NONE', *, *, #6638, .T. ) ;
#5703 = DIRECTION ( 'NONE',  ( 0.000000000000000000, 0.000000000000000000, 1.000000000000000000 ) ) ;
#5704 = AXIS2_PLACEMENT_3D ( 'NONE', #6355, #2658, #616 ) ;
#5705 = CARTESIAN_POINT ( 'NONE',  ( 2.344047193898588954, 3.265465875126466688, 1.943940613948618539E-16 ) ) ;
#5706 = CARTESIAN_POINT ( 'NONE',  ( 0.000000000000000000, 0.000000000000000000, 13.00000000000000178 ) ) ;
#5707 = CYLINDRICAL_SURFACE ( 'NONE', #3465, 3.000000000000002665 ) ;
#5708 = EDGE_CURVE ( 'NONE', #1445, #13430, #11526, .T. ) ;
#5709 = PLANE ( 'NONE',  #14283 ) ;
#5710 = AXIS2_PLACEMENT_3D ( 'NONE', #6794, #11680, #11457 ) ;
#5711 = LINE ( 'NONE', #4798, #8523 ) ;
#5712 = AXIS2_PLACEMENT_3D ( 'NONE', #8871, #5238, #7430 ) ;
#5713 = EDGE_LOOP ( 'NONE', ( #3683, #10600, #13712, #8408 ) ) ;
#5714 = CARTESIAN_POINT ( 'NONE',  ( 5.000000000000007994, 5.204748896376217172E-16, -4.249999999999972466 ) ) ;
#5715 = CARTESIAN_POINT ( 'NONE',  ( 7.787692492290230639, 94.68070094645281642, -20.00000000000000355 ) ) ;
#5716 = DIRECTION ( 'NONE',  ( -0.000000000000000000, -0.000000000000000000, 1.000000000000000000 ) ) ;
#5717 = DIRECTION ( 'NONE',  ( -1.000000000000000000, -4.625929269271481378E-15, 0.000000000000000000 ) ) ;
#5718 = ORIENTED_EDGE ( 'NONE', *, *, #10613, .T. ) ;
#5719 = AXIS2_PLACEMENT_3D ( 'NONE', #11443, #5660, #13793 ) ;
#5720 = CYLINDRICAL_SURFACE ( 'NONE', #11196, 3.000000000000002665 ) ;
#5721 = EDGE_LOOP ( 'NONE', ( #14078, #7150, #10060, #4284 ) ) ;
#5722 = EDGE_CURVE ( 'NONE', #12796, #14448, #2399, .T. ) ;
#5723 = DIRECTION ( 'NONE',  ( 1.000000000000000000, 0.000000000000000000, 0.000000000000000000 ) ) ;
#5724 = EDGE_CURVE ( 'NONE', #9289, #7921, #8107, .T. ) ;
#5725 = DIRECTION ( 'NONE',  ( -0.000000000000000000, -0.000000000000000000, -1.000000000000000000 ) ) ;
#5726 = CARTESIAN_POINT ( 'NONE',  ( -11.55014193876141171, 53.26842454702440222, -13.00000000000000178 ) ) ;
#5727 = ORIENTED_EDGE ( 'NONE', *, *, #13393, .F. ) ;
#5728 = ORIENTED_EDGE ( 'NONE', *, *, #8053, .T. ) ;
#5729 = ORIENTED_EDGE ( 'NONE', *, *, #10091, .F. ) ;
#5730 = VERTEX_POINT ( 'NONE', #14177 ) ;
#5731 = AXIS2_PLACEMENT_3D ( 'NONE', #10635, #9495, #5097 ) ;
#5732 = CARTESIAN_POINT ( 'NONE',  ( -7.500000000000000888, 62.55197838597913318, -20.00000000000000000 ) ) ;
#5733 = DIRECTION ( 'NONE',  ( 1.000000000000000000, 0.000000000000000000, 0.000000000000000000 ) ) ;
#5734 = DIRECTION ( 'NONE',  ( -1.000000000000000000, 0.000000000000000000, 0.000000000000000000 ) ) ;
#5735 = ORIENTED_EDGE ( 'NONE', *, *, #206, .F. ) ;
#5736 = ORIENTED_EDGE ( 'NONE', *, *, #1563, .F. ) ;
#5737 = EDGE_CURVE ( 'NONE', #7405, #9994, #8543, .T. ) ;
#5738 = ORIENTED_EDGE ( 'NONE', *, *, #10712, .T. ) ;
#5739 = EDGE_CURVE ( 'NONE', #3649, #12421, #6188, .T. ) ;
#5740 = CIRCLE ( 'NONE', #4540, 60.50000000000000000 ) ;
#5741 = DIRECTION ( 'NONE',  ( -0.000000000000000000, -0.000000000000000000, 1.000000000000000000 ) ) ;
#5742 = DIRECTION ( 'NONE',  ( -0.000000000000000000, -0.000000000000000000, 1.000000000000000000 ) ) ;
#5743 = DIRECTION ( 'NONE',  ( -1.000000000000000000, 0.000000000000000000, 0.000000000000000000 ) ) ;
#5744 = DIRECTION ( 'NONE',  ( -0.000000000000000000, -0.000000000000000000, -1.000000000000000000 ) ) ;
#5745 = ORIENTED_EDGE ( 'NONE', *, *, #4408, .F. ) ;
#5746 = CARTESIAN_POINT ( 'NONE',  ( -12.86891638962156215, 56.43380494353993271, -10.50000000000000000 ) ) ;
#5747 = ORIENTED_EDGE ( 'NONE', *, *, #7773, .F. ) ;
#5748 = EDGE_CURVE ( 'NONE', #3199, #9900, #10045, .T. ) ;
#5749 = CARTESIAN_POINT ( 'NONE',  ( 37.12029293941315444, -89.61631465359504034, 8.000000000000000000 ) ) ;
#5750 = DIRECTION ( 'NONE',  ( -0.000000000000000000, -0.000000000000000000, -1.000000000000000000 ) ) ;
#5751 = EDGE_LOOP ( 'NONE', ( #13791, #5303, #609, #6112 ) ) ;
#5752 = ORIENTED_EDGE ( 'NONE', *, *, #12228, .F. ) ;
#5753 = DIRECTION ( 'NONE',  ( 0.000000000000000000, 0.000000000000000000, -1.000000000000000000 ) ) ;
#5754 = VERTEX_POINT ( 'NONE', #2788 ) ;
#5755 = ADVANCED_FACE ( 'NONE', ( #5059 ), #3930, .T. ) ;
#5756 = VERTEX_POINT ( 'NONE', #11987 ) ;
#5757 = CARTESIAN_POINT ( 'NONE',  ( 5.204748896376250896E-15, 85.00000000000000000, 46.00000000000000000 ) ) ;
#5758 = CARTESIAN_POINT ( 'NONE',  ( -31.76435573746199381, 42.04772703543562073, 10.49999999999999822 ) ) ;
#5759 = FACE_OUTER_BOUND ( 'NONE', #5620, .T. ) ;
#5760 = CARTESIAN_POINT ( 'NONE',  ( -1.257172072275683394, 3.892973519170756180, -3.433252694550406048 ) ) ;
#5761 = DIRECTION ( 'NONE',  ( -1.000000000000000000, 0.000000000000000000, 0.000000000000000000 ) ) ;
#5762 = VERTEX_POINT ( 'NONE', #3787 ) ;
#5763 = DIRECTION ( 'NONE',  ( -0.000000000000000000, -0.000000000000000000, 1.000000000000000000 ) ) ;
#5764 = CARTESIAN_POINT ( 'NONE',  ( 0.000000000000000000, 0.000000000000000000, -10.50000000000000000 ) ) ;
#5765 = EDGE_LOOP ( 'NONE', ( #14775, #6222, #2863, #8209 ) ) ;
#5766 = DIRECTION ( 'NONE',  ( -1.000000000000000000, 0.000000000000000000, 0.000000000000000000 ) ) ;
#5767 = CYLINDRICAL_SURFACE ( 'NONE', #12489, 0.5000000000000004441 ) ;
#5768 = CARTESIAN_POINT ( 'NONE',  ( 32.26435573746228158, -42.04772703543541468, 8.000000000000000000 ) ) ;
#5769 = DIRECTION ( 'NONE',  ( -1.000000000000000000, 0.000000000000000000, 0.000000000000000000 ) ) ;
#5770 = DIRECTION ( 'NONE',  ( -0.000000000000000000, -0.000000000000000000, 1.000000000000000000 ) ) ;
#5771 = CARTESIAN_POINT ( 'NONE',  ( -34.44830544488820578, 94.94374256356071839, 16.00000000000000000 ) ) ;
#5772 = EDGE_CURVE ( 'NONE', #12974, #13772, #9667, .T. ) ;
#5773 = CARTESIAN_POINT ( 'NONE',  ( 0.000000000000000000, 0.000000000000000000, -16.00000000000000000 ) ) ;
#5774 = ADVANCED_FACE ( 'NONE', ( #10601 ), #14252, .T. ) ;
#5775 = CARTESIAN_POINT ( 'NONE',  ( 5.204748896376250896E-15, 85.00000000000000000, 31.00000000000000000 ) ) ;
#5776 = EDGE_CURVE ( 'NONE', #8180, #5501, #14433, .T. ) ;
#5777 = VERTEX_POINT ( 'NONE', #2857 ) ;
#5778 = CARTESIAN_POINT ( 'NONE',  ( 2.500000000000002220, 1.768423874527823347, -1.021000000000001018 ) ) ;
#5779 = DIRECTION ( 'NONE',  ( 0.000000000000000000, 0.000000000000000000, 1.000000000000000000 ) ) ;
#5780 = DIRECTION ( 'NONE',  ( 1.000000000000000000, 0.000000000000000000, 0.000000000000000000 ) ) ;
#5781 = ADVANCED_FACE ( 'NONE', ( #14318 ), #12057, .F. ) ;
#5782 = FACE_OUTER_BOUND ( 'NONE', #2966, .T. ) ;
#5783 = ORIENTED_EDGE ( 'NONE', *, *, #1875, .T. ) ;
#5784 = DIRECTION ( 'NONE',  ( 1.000000000000000000, 0.000000000000000000, 0.000000000000000000 ) ) ;
#5785 = ORIENTED_EDGE ( 'NONE', *, *, #13538, .T. ) ;
#5786 = EDGE_CURVE ( 'NONE', #7296, #14250, #12250, .T. ) ;
#5787 = CARTESIAN_POINT ( 'NONE',  ( -30.80502811811232888, -49.00442420935981147, -13.00000000000000178 ) ) ;
#5788 = FACE_OUTER_BOUND ( 'NONE', #2835, .T. ) ;
#5789 = DIRECTION ( 'NONE',  ( 0.000000000000000000, 0.000000000000000000, 1.000000000000000000 ) ) ;
#5790 = DIRECTION ( 'NONE',  ( 0.000000000000000000, 0.000000000000000000, 1.000000000000000000 ) ) ;
#5791 = EDGE_CURVE ( 'NONE', #11551, #13490, #9811, .T. ) ;
#5792 = EDGE_LOOP ( 'NONE', ( #2997, #5475, #12148 ) ) ;
#5793 = CARTESIAN_POINT ( 'NONE',  ( -11.47656068366043236, 61.94660012053729048, -18.08543280684388677 ) ) ;
#5794 = MECHANICAL_DESIGN_GEOMETRIC_PRESENTATION_REPRESENTATION (  '', ( #5077 ), #14545 ) ;
#5795 = LINE ( 'NONE', #13870, #608 ) ;
#5796 = CARTESIAN_POINT ( 'NONE',  ( 0.000000000000000000, 0.000000000000000000, 8.000000000000000000 ) ) ;
#5797 = ORIENTED_EDGE ( 'NONE', *, *, #12138, .F. ) ;
#5798 = CIRCLE ( 'NONE', #1209, 5.000000000000001776 ) ;
#5799 = ORIENTED_EDGE ( 'NONE', *, *, #2576, .T. ) ;
#5800 = ORIENTED_EDGE ( 'NONE', *, *, #7393, .T. ) ;
#5801 = DIRECTION ( 'NONE',  ( 1.000000000000000000, 0.000000000000000000, 0.000000000000000000 ) ) ;
#5802 = AXIS2_PLACEMENT_3D ( 'NONE', #6083, #10868, #14367 ) ;
#5803 = CARTESIAN_POINT ( 'NONE',  ( -50.00000000000000000, 0.000000000000000000, -8.000000000000000000 ) ) ;
#5804 = CARTESIAN_POINT ( 'NONE',  ( 0.000000000000000000, 0.000000000000000000, -31.00000000000000000 ) ) ;
#5805 = SHAPE_REPRESENTATION_RELATIONSHIP ( 'NONE' , 'NONE' ,  #1232, #2214 ) ;
#5806 = AXIS2_PLACEMENT_3D ( 'NONE', #11660, #12859, #31 ) ;
#5807 = CARTESIAN_POINT ( 'NONE',  ( 51.19406879332056093, 13.71740939043382745, 10.49999999999999822 ) ) ;
#5808 = VECTOR ( 'NONE', #7448, 1000.000000000000000 ) ;
#5809 = CARTESIAN_POINT ( 'NONE',  ( -2.449293598294708880E-16, 38.00000000000000000, -25.50000000000000355 ) ) ;
#5810 = VERTEX_POINT ( 'NONE', #10899 ) ;
#5811 = AXIS2_PLACEMENT_3D ( 'NONE', #7809, #4035, #8646 ) ;
#5812 = VERTEX_POINT ( 'NONE', #2710 ) ;
#5813 = CARTESIAN_POINT ( 'NONE',  ( 0.000000000000000000, 0.000000000000000000, 8.000000000000000000 ) ) ;
#5815 = EDGE_CURVE ( 'NONE', #9297, #6889, #1581, .T. ) ;
#5814 = DIRECTION ( 'NONE',  ( -1.000000000000000000, 0.000000000000000000, 0.000000000000000000 ) ) ;
#5816 = EDGE_CURVE ( 'NONE', #9608, #1839, #7244, .T. ) ;
#5817 = EDGE_LOOP ( 'NONE', ( #7340, #5834, #9517, #11870, #8013 ) ) ;
#5818 = VECTOR ( 'NONE', #8055, 1000.000000000000000 ) ;
#5819 = EDGE_CURVE ( 'NONE', #13345, #14403, #5211, .T. ) ;
#5820 = ORIENTED_EDGE ( 'NONE', *, *, #1248, .F. ) ;
#5821 = FACE_OUTER_BOUND ( 'NONE', #9284, .T. ) ;
#5822 = CIRCLE ( 'NONE', #7763, 0.5000000000000022204 ) ;
#5823 = ORIENTED_EDGE ( 'NONE', *, *, #2963, .F. ) ;
#5824 = VERTEX_POINT ( 'NONE', #199 ) ;
#5825 = CIRCLE ( 'NONE', #7766, 63.00000000000000000 ) ;
#5826 = DIRECTION ( 'NONE',  ( -1.000000000000000000, 0.000000000000000000, 0.000000000000000000 ) ) ;
#5827 = EDGE_CURVE ( 'NONE', #12589, #7227, #14101, .T. ) ;
#5828 = DIRECTION ( 'NONE',  ( 1.000000000000000000, 0.000000000000000000, 0.000000000000000000 ) ) ;
#5829 = DIRECTION ( 'NONE',  ( -0.000000000000000000, -0.000000000000000000, -1.000000000000000000 ) ) ;
#5830 = CYLINDRICAL_SURFACE ( 'NONE', #11656, 63.00000000000000000 ) ;
#5831 = CIRCLE ( 'NONE', #1724, 100.0000000000000000 ) ;
#5832 = VECTOR ( 'NONE', #3187, 1000.000000000000000 ) ;
#5833 = CARTESIAN_POINT ( 'NONE',  ( 71.58935777509475429, -68.58935777509547904, 8.000000000000000000 ) ) ;
#5834 = ORIENTED_EDGE ( 'NONE', *, *, #7365, .T. ) ;
#5835 = VECTOR ( 'NONE', #4468, 1000.000000000000000 ) ;
#5836 = CARTESIAN_POINT ( 'NONE',  ( -33.49014761921588956, 11.74264578624790190, -28.00000000000000000 ) ) ;
#5837 = VERTEX_POINT ( 'NONE', #8323 ) ;
#5838 = EDGE_CURVE ( 'NONE', #12802, #23, #12964, .T. ) ;
#5839 = DIRECTION ( 'NONE',  ( -0.000000000000000000, -0.000000000000000000, 1.000000000000000000 ) ) ;
#5840 = EDGE_LOOP ( 'NONE', ( #1880, #3693 ) ) ;
#5841 = DIRECTION ( 'NONE',  ( 0.000000000000000000, 0.000000000000000000, 1.000000000000000000 ) ) ;
#5842 = AXIS2_PLACEMENT_3D ( 'NONE', #5231, #6427, #14492 ) ;
#5843 = DIRECTION ( 'NONE',  ( 0.000000000000000000, 0.000000000000000000, 1.000000000000000000 ) ) ;
#5844 = LINE ( 'NONE', #10483, #7024 ) ;
#5845 = AXIS2_PLACEMENT_3D ( 'NONE', #2904, #7521, #12039 ) ;
#5846 = AXIS2_PLACEMENT_3D ( 'NONE', #1922, #7768, #6699 ) ;
#5847 = DIRECTION ( 'NONE',  ( 0.000000000000000000, 0.000000000000000000, -1.000000000000000000 ) ) ;
#5848 = DIRECTION ( 'NONE',  ( -1.000000000000000000, 0.000000000000000000, 0.000000000000000000 ) ) ;
#5849 = DIRECTION ( 'NONE',  ( -0.000000000000000000, -0.000000000000000000, 1.000000000000000000 ) ) ;
#5850 = CARTESIAN_POINT ( 'NONE',  ( -3.999999999999998224, 0.8730739991738329930, -3.223134629628430226 ) ) ;
#5851 = CONTEXT_DEPENDENT_SHAPE_REPRESENTATION ( #7550, #14594 ) ;
#5852 = DIRECTION ( 'NONE',  ( -1.000000000000000000, 0.000000000000000000, 0.000000000000000000 ) ) ;
#5853 = AXIS2_PLACEMENT_3D ( 'NONE', #7093, #2907, #6302 ) ;
#5854 = ORIENTED_EDGE ( 'NONE', *, *, #12793, .F. ) ;
#5855 = B_SPLINE_CURVE_WITH_KNOTS ( 'NONE', 3,
 ( #3055, #8808, #3197, #9028, #6676, #7671, #12315, #8726 ),
 .UNSPECIFIED., .F., .F.,
 ( 4, 2, 2, 4 ),
 ( 0.000000000000000000, 0.002450665683189820129, 0.003675998524784729327, 0.004901331366379639391 ),
 .UNSPECIFIED. ) ;
#5856 = CARTESIAN_POINT ( 'NONE',  ( -10.80358476664834910, 106.4534462909512769, -18.76728514983857465 ) ) ;
#5857 = DIRECTION ( 'NONE',  ( 0.000000000000000000, 0.000000000000000000, 1.000000000000000000 ) ) ;
#5858 = AXIS2_PLACEMENT_3D ( 'NONE', #4487, #991, #9103 ) ;
#5859 = DIRECTION ( 'NONE',  ( 1.000000000000000000, 0.000000000000000000, 0.000000000000000000 ) ) ;
#5860 = DIRECTION ( 'NONE',  ( 1.000000000000000000, 0.000000000000000000, 0.000000000000000000 ) ) ;
#5861 = ORIENTED_EDGE ( 'NONE', *, *, #12371, .T. ) ;
#5862 = EDGE_CURVE ( 'NONE', #1935, #4441, #3036, .T. ) ;
#5863 = CARTESIAN_POINT ( 'NONE',  ( 0.000000000000000000, 0.000000000000000000, -31.00000000000000000 ) ) ;
#5864 = ORIENTED_EDGE ( 'NONE', *, *, #348, .F. ) ;
#5865 = DIRECTION ( 'NONE',  ( 0.000000000000000000, 0.000000000000000000, 1.000000000000000000 ) ) ;
#5866 = CARTESIAN_POINT ( 'NONE',  ( -22.05882352941176450, 71.68269180561142662, 16.00000000000000000 ) ) ;
#5867 = DIRECTION ( 'NONE',  ( 0.000000000000000000, 0.000000000000000000, 1.000000000000000000 ) ) ;
#5868 = AXIS2_PLACEMENT_3D ( 'NONE', #4123, #8818, #7520 ) ;
#5869 = DIRECTION ( 'NONE',  ( 0.000000000000000000, 0.000000000000000000, 1.000000000000000000 ) ) ;
#5870 = VERTEX_POINT ( 'NONE', #6245 ) ;
#5871 = DIRECTION ( 'NONE',  ( 1.000000000000000000, 0.000000000000000000, 0.000000000000000000 ) ) ;
#5872 = CARTESIAN_POINT ( 'NONE',  ( -34.44830544488820578, 94.94374256356073261, -16.00000000000000000 ) ) ;
#5873 = VECTOR ( 'NONE', #8163, 1000.000000000000000 ) ;
#5874 = DIRECTION ( 'NONE',  ( 0.000000000000000000, 0.000000000000000000, -1.000000000000000000 ) ) ;
#5875 = VERTEX_POINT ( 'NONE', #3996 ) ;
#5876 = VERTEX_POINT ( 'NONE', #8459 ) ;
#5877 = EDGE_CURVE ( 'NONE', #7439, #14780, #1487, .T. ) ;
#5878 = EDGE_CURVE ( 'NONE', #8551, #6323, #368, .T. ) ;
#5879 = AXIS2_PLACEMENT_3D ( 'NONE', #3621, #13801, #12807 ) ;
#5880 = ORIENTED_EDGE ( 'NONE', *, *, #3255, .T. ) ;
#5881 = CARTESIAN_POINT ( 'NONE',  ( 36.52608637591580987, -92.55687898036916295, -13.00000000000000178 ) ) ;
#5882 = AXIS2_PLACEMENT_3D ( 'NONE', #14221, #9498, #4806 ) ;
#5883 = DIRECTION ( 'NONE',  ( 0.000000000000000000, 0.000000000000000000, 1.000000000000000000 ) ) ;
#5884 = CARTESIAN_POINT ( 'NONE',  ( 4.175002511812153649, 2.208363329454889890, -3.469254087858246294 ) ) ;
#5885 =( NAMED_UNIT ( * ) PLANE_ANGLE_UNIT ( ) SI_UNIT ( $, .RADIAN. ) );
#5886 = CARTESIAN_POINT ( 'NONE',  ( -30.80502811811232888, -49.00442420935981147, -13.00000000000000178 ) ) ;
#5887 = CARTESIAN_POINT ( 'NONE',  ( -33.48561063518626923, 47.21331623427104063, 8.000000000000000000 ) ) ;
#5888 = AXIS2_PLACEMENT_3D ( 'NONE', #10796, #2827, #7508 ) ;
#5889 = VERTEX_POINT ( 'NONE', #2701 ) ;
#5890 = DIRECTION ( 'NONE',  ( 0.000000000000000000, 0.000000000000000000, 1.000000000000000000 ) ) ;
#5891 = FACE_OUTER_BOUND ( 'NONE', #4833, .T. ) ;
#5892 = CIRCLE ( 'NONE', #9045, 17.00000000000000000 ) ;
#5893 = VERTEX_POINT ( 'NONE', #9824 ) ;
#5894 = CIRCLE ( 'NONE', #14146, 4.000000000000000000 ) ;
#5895 = EDGE_LOOP ( 'NONE', ( #12402, #39, #6499, #4308, #10141, #12752 ) ) ;
#5896 = DIRECTION ( 'NONE',  ( -0.000000000000000000, -0.000000000000000000, 1.000000000000000000 ) ) ;
#5897 = ORIENTED_EDGE ( 'NONE', *, *, #13274, .F. ) ;
#5898 = VERTEX_POINT ( 'NONE', #13182 ) ;
#5899 = AXIS2_PLACEMENT_3D ( 'NONE', #8956, #7597, #7512 ) ;
#5900 = DIRECTION ( 'NONE',  ( 1.000000000000000000, 0.000000000000000000, 0.000000000000000000 ) ) ;
#5901 = CYLINDRICAL_SURFACE ( 'NONE', #2467, 60.50000000000000000 ) ;
#5902 = CIRCLE ( 'NONE', #7109, 60.50000000000000000 ) ;
#5903 = EDGE_CURVE ( 'NONE', #7149, #2085, #14469, .T. ) ;
#5904 = DIRECTION ( 'NONE',  ( 0.000000000000000000, 0.000000000000000000, -1.000000000000000000 ) ) ;
#5905 = DIRECTION ( 'NONE',  ( 1.000000000000000000, 0.000000000000000000, 0.000000000000000000 ) ) ;
#5906 = CARTESIAN_POINT ( 'NONE',  ( 92.61631465359491244, 37.12029293941346708, -8.000000000000000000 ) ) ;
#5907 = EDGE_CURVE ( 'NONE', #571, #14147, #14186, .T. ) ;
#5908 = ORIENTED_EDGE ( 'NONE', *, *, #2182, .F. ) ;
#5909 = CARTESIAN_POINT ( 'NONE',  ( 5.204748896376250896E-15, 85.00000000000000000, 46.00000000000000000 ) ) ;
#5910 = VECTOR ( 'NONE', #2445, 1000.000000000000000 ) ;
#5911 = CIRCLE ( 'NONE', #14408, 60.50000000000000711 ) ;
#5912 = CIRCLE ( 'NONE', #561, 3.000000000000002665 ) ;
#5913 = EDGE_CURVE ( 'NONE', #7348, #4331, #12051, .T. ) ;
#5914 = CIRCLE ( 'NONE', #7855, 3.000000000000002665 ) ;
#5915 = ORIENTED_EDGE ( 'NONE', *, *, #6517, .F. ) ;
#5916 = DIRECTION ( 'NONE',  ( -0.000000000000000000, -0.000000000000000000, 1.000000000000000000 ) ) ;
#5917 = EDGE_LOOP ( 'NONE', ( #10680, #3935, #13780, #1921, #5153 ) ) ;
#5918 = DIRECTION ( 'NONE',  ( 1.000000000000000000, 0.000000000000000000, 0.000000000000000000 ) ) ;
#5919 = ADVANCED_FACE ( 'NONE', ( #11893 ), #7397, .F. ) ;
#5920 = VECTOR ( 'NONE', #2372, 1000.000000000000000 ) ;
#5921 = ADVANCED_FACE ( 'NONE', ( #10822 ), #14309, .T. ) ;
#5922 = DIRECTION ( 'NONE',  ( -0.000000000000000000, -0.000000000000000000, -1.000000000000000000 ) ) ;
#5923 = CARTESIAN_POINT ( 'NONE',  ( -9.714076971208447375, 106.5585699559772479, 19.49498877141798658 ) ) ;
#5924 = DIRECTION ( 'NONE',  ( -1.000000000000000000, 0.000000000000000000, 0.000000000000000000 ) ) ;
#5925 = CIRCLE ( 'NONE', #10774, 0.5000000000000073275 ) ;
#5926 = AXIS2_PLACEMENT_3D ( 'NONE', #9219, #11666, #3380 ) ;
#5927 = AXIS2_PLACEMENT_3D ( 'NONE', #9154, #4682, #1189 ) ;
#5928 = FACE_OUTER_BOUND ( 'NONE', #1350, .T. ) ;
#5929 = DIRECTION ( 'NONE',  ( 1.000000000000000000, 5.329070518200751394E-15, 0.000000000000000000 ) ) ;
#5930 = ORIENTED_EDGE ( 'NONE', *, *, #3100, .T. ) ;
#5931 = EDGE_CURVE ( 'NONE', #9955, #1777, #2305, .T. ) ;
#5932 = CARTESIAN_POINT ( 'NONE',  ( 0.000000000000000000, 4.618802153517009401, -0.5000000000000004441 ) ) ;
#5933 = LINE ( 'NONE', #14914, #4691 ) ;
#5934 = AXIS2_PLACEMENT_3D ( 'NONE', #5621, #3200, #14820 ) ;
#5935 = DIRECTION ( 'NONE',  ( 0.000000000000000000, 0.000000000000000000, 1.000000000000000000 ) ) ;
#5936 = CIRCLE ( 'NONE', #119, 3.000000000000002665 ) ;
#5937 = AXIS2_PLACEMENT_3D ( 'NONE', #5626, #7682, #4206 ) ;
#5938 = CARTESIAN_POINT ( 'NONE',  ( -56.43380494354004639, -12.86891638962099549, -10.50000000000000000 ) ) ;
#5939 = ORIENTED_EDGE ( 'NONE', *, *, #13742, .T. ) ;
#5940 = CARTESIAN_POINT ( 'NONE',  ( 12.50000000000000000, 100.2235002382176248, 15.00000000000000000 ) ) ;
#5941 = ORIENTED_EDGE ( 'NONE', *, *, #6210, .F. ) ;
#5942 = CARTESIAN_POINT ( 'NONE',  ( -2.345747346278107770, 3.264484291692488771, -0.01223254789873306179 ) ) ;
#5943 = CARTESIAN_POINT ( 'NONE',  ( -3.999999999999996447, 1.941961291383474952, -0.3515519931180187685 ) ) ;
#5944 = MECHANICAL_DESIGN_GEOMETRIC_PRESENTATION_REPRESENTATION (  '', ( #7888 ), #1601 ) ;
#5945 = DIRECTION ( 'NONE',  ( -1.000000000000000000, -1.198854274490189999E-13, 0.000000000000000000 ) ) ;
#5946 = CARTESIAN_POINT ( 'NONE',  ( -37.12029293941441210, -89.61631465359452875, -8.000000000000000000 ) ) ;
#5947 = VERTEX_POINT ( 'NONE', #6181 ) ;
#5948 = DIRECTION ( 'NONE',  ( -1.000000000000000000, 0.000000000000000000, 0.000000000000000000 ) ) ;
#5949 = FACE_OUTER_BOUND ( 'NONE', #7384, .T. ) ;
#5950 = CARTESIAN_POINT ( 'NONE',  ( 33.48561063518626923, -47.21331623427104063, -13.00000000000000178 ) ) ;
#5951 = VERTEX_POINT ( 'NONE', #491 ) ;
#5952 = AXIS2_PLACEMENT_3D ( 'NONE', #8033, #4625, #3713 ) ;
#5953 = VERTEX_POINT ( 'NONE', #5052 ) ;
#5954 = VERTEX_POINT ( 'NONE', #6317 ) ;
#5955 = DIRECTION ( 'NONE',  ( -1.000000000000000000, 0.000000000000000000, 0.000000000000000000 ) ) ;
#5956 = CYLINDRICAL_SURFACE ( 'NONE', #8031, 63.00000000000000000 ) ;
#5957 = CARTESIAN_POINT ( 'NONE',  ( 0.000000000000000000, 0.000000000000000000, -25.50000000000000355 ) ) ;
#5958 = CARTESIAN_POINT ( 'NONE',  ( 47.00000000000001421, 81.24038404635960831, -16.00000000000000000 ) ) ;
#5959 = CIRCLE ( 'NONE', #7173, 3.000000000000002665 ) ;
#5960 = EDGE_CURVE ( 'NONE', #914, #11061, #4741, .T. ) ;
#5961 = ORIENTED_EDGE ( 'NONE', *, *, #8522, .F. ) ;
#5962 = VERTEX_POINT ( 'NONE', #13319 ) ;
#5963 = ADVANCED_FACE ( 'NONE', ( #14389 ), #13103, .F. ) ;
#5964 = SHAPE_REPRESENTATION ( 'brake pad', ( #5108 ), #2434 ) ;
#5965 = ADVANCED_FACE ( 'NONE', ( #9521 ), #10745, .F. ) ;
#5966 = ORIENTED_EDGE ( 'NONE', *, *, #3569, .F. ) ;
#5967 = EDGE_CURVE ( 'NONE', #12052, #11984, #607, .T. ) ;
#5968 = DIRECTION ( 'NONE',  ( 1.000000000000000000, 0.000000000000000000, 0.000000000000000000 ) ) ;
#5969 = CYLINDRICAL_SURFACE ( 'NONE', #7455, 60.50000000000000000 ) ;
#5970 = CARTESIAN_POINT ( 'NONE',  ( 7.383907457638312799, 52.72775723226772726, -13.00000000000000178 ) ) ;
#5971 = VERTEX_POINT ( 'NONE', #1564 ) ;
#5972 = ORIENTED_EDGE ( 'NONE', *, *, #13417, .T. ) ;
#5973 = CARTESIAN_POINT ( 'NONE',  ( -12.86891638962156215, 56.43380494353993271, 8.000000000000000000 ) ) ;
#5974 = AXIS2_PLACEMENT_3D ( 'NONE', #5317, #695, #8725 ) ;
#5975 = EDGE_LOOP ( 'NONE', ( #832, #2142, #3274, #11881, #2800 ) ) ;
#5976 = DIRECTION ( 'NONE',  ( 1.000000000000000000, 0.000000000000000000, 0.000000000000000000 ) ) ;
#5977 = CARTESIAN_POINT ( 'NONE',  ( -7.500000000000000888, 74.62405778299650194, 20.00000000000000000 ) ) ;
#5978 = DIRECTION ( 'NONE',  ( -1.000000000000000000, 0.000000000000000000, 0.000000000000000000 ) ) ;
#5979 = DIRECTION ( 'NONE',  ( 1.000000000000000000, 0.000000000000000000, 0.000000000000000000 ) ) ;
#5980 = CARTESIAN_POINT ( 'NONE',  ( 22.33583958711425055, -30.74264578624780597, 14.49999999999999822 ) ) ;
#5981 = DIRECTION ( 'NONE',  ( -1.000000000000000000, 0.000000000000000000, 0.000000000000000000 ) ) ;
#5982 = ORIENTED_EDGE ( 'NONE', *, *, #7977, .T. ) ;
#5983 = EDGE_CURVE ( 'NONE', #6726, #13811, #2064, .T. ) ;
#5984 = CARTESIAN_POINT ( 'NONE',  ( -4.000000000000000000, -7.155734338404329264E-15, -3.142992957459235015 ) ) ;
#5985 = ORIENTED_EDGE ( 'NONE', *, *, #12293, .F. ) ;
#5986 = CARTESIAN_POINT ( 'NONE',  ( -3.240162412667121864E-13, -4.796980096169331631, -3.721999068284310042 ) ) ;
#5987 = CARTESIAN_POINT ( 'NONE',  ( -27.94117647058823550, 90.79807628710781842, -23.50000000000000000 ) ) ;
#5988 = VERTEX_POINT ( 'NONE', #3920 ) ;
#5989 = CARTESIAN_POINT ( 'NONE',  ( 25.00000000000000000, 81.24038404635960831, 23.50000000000000355 ) ) ;
#5990 = CLOSED_SHELL ( 'NONE', ( #1995, #14046, #13063, #3235, #1168, #8390, #5278 ) ) ;
#5991 = FACE_OUTER_BOUND ( 'NONE', #9621, .T. ) ;
#5992 = DIRECTION ( 'NONE',  ( 0.000000000000000000, 0.000000000000000000, 1.000000000000000000 ) ) ;
#5993 = CARTESIAN_POINT ( 'NONE',  ( -49.00442420935969778, 30.80502811811250297, 10.49999999999999822 ) ) ;
#5994 = CARTESIAN_POINT ( 'NONE',  ( 89.61631465359468507, -37.12029293941410657, 10.49999999999999822 ) ) ;
#5995 = ORIENTED_EDGE ( 'NONE', *, *, #4698, .T. ) ;
#5996 = DIRECTION ( 'NONE',  ( 1.000000000000000000, 0.000000000000000000, 0.000000000000000000 ) ) ;
#5997 = VERTEX_POINT ( 'NONE', #14244 ) ;
#5998 = CARTESIAN_POINT ( 'NONE',  ( 37.02125851216354846, -90.10640870805738700, -13.00000000000000178 ) ) ;
#5999 = CARTESIAN_POINT ( 'NONE',  ( 5.204748896376250896E-15, 85.00000000000000000, 46.00000000000000000 ) ) ;
#6000 = ADVANCED_FACE ( 'NONE', ( #7318 ), #13544, .F. ) ;
#6001 = VECTOR ( 'NONE', #1200, 1000.000000000000000 ) ;
#6002 = ADVANCED_FACE ( 'NONE', ( #7697 ), #6768, .F. ) ;
#6003 = DIRECTION ( 'NONE',  ( 1.000000000000000000, 0.000000000000000000, 0.000000000000000000 ) ) ;
#6004 = DIRECTION ( 'NONE',  ( 0.000000000000000000, 0.000000000000000000, -1.000000000000000000 ) ) ;
#6005 = EDGE_CURVE ( 'NONE', #8680, #198, #5936, .T. ) ;
#6006 = ORIENTED_EDGE ( 'NONE', *, *, #2694, .F. ) ;
#6007 = CARTESIAN_POINT ( 'NONE',  ( 53.26842454702428142, 11.55014193876197126, -8.000000000000000000 ) ) ;
#6008 = ORIENTED_EDGE ( 'NONE', *, *, #3021, .F. ) ;
#6009 = ORIENTED_EDGE ( 'NONE', *, *, #5645, .F. ) ;
#6010 = CARTESIAN_POINT ( 'NONE',  ( 0.000000000000000000, 0.000000000000000000, -13.00000000000000178 ) ) ;
#6011 = DIRECTION ( 'NONE',  ( 1.000000000000000000, 0.000000000000000000, 0.000000000000000000 ) ) ;
#6012 = EDGE_CURVE ( 'NONE', #11617, #12937, #8599, .T. ) ;
#6013 = DIRECTION ( 'NONE',  ( 1.000000000000000000, 0.000000000000000000, 0.000000000000000000 ) ) ;
#6014 = LINE ( 'NONE', #2688, #6136 ) ;
#6015 = EDGE_LOOP ( 'NONE', ( #12579, #116, #2466, #10217 ) ) ;
#6016 = DIRECTION ( 'NONE',  ( 0.000000000000000000, 0.000000000000000000, 1.000000000000000000 ) ) ;
#6017 = DIRECTION ( 'NONE',  ( -1.000000000000000000, 0.000000000000000000, 0.000000000000000000 ) ) ;
#6018 = EDGE_CURVE ( 'NONE', #143, #13983, #11289, .T. ) ;
#6019 = LINE ( 'NONE', #9590, #4194 ) ;
#6020 = ORIENTED_EDGE ( 'NONE', *, *, #1398, .F. ) ;
#6021 = AXIS2_PLACEMENT_3D ( 'NONE', #12157, #7435, #1452 ) ;
#6022 = ORIENTED_EDGE ( 'NONE', *, *, #11662, .F. ) ;
#6023 = DIRECTION ( 'NONE',  ( 0.000000000000000000, 0.000000000000000000, -1.000000000000000000 ) ) ;
#6024 = DIRECTION ( 'NONE',  ( 0.000000000000000000, 0.000000000000000000, 1.000000000000000000 ) ) ;
#6025 = FACE_BOUND ( 'NONE', #3093, .T. ) ;
#6026 = CARTESIAN_POINT ( 'NONE',  ( -29.95643228365058164, 96.45524571768991962, -12.60642518152332237 ) ) ;
#6027 = ORIENTED_EDGE ( 'NONE', *, *, #6611, .T. ) ;
#6028 = ORIENTED_EDGE ( 'NONE', *, *, #1988, .T. ) ;
#6029 = ORIENTED_EDGE ( 'NONE', *, *, #10659, .F. ) ;
#6030 = DIRECTION ( 'NONE',  ( -0.7071067811865479058, 0.000000000000000000, 0.7071067811865472397 ) ) ;
#6031 = VECTOR ( 'NONE', #11858, 1000.000000000000000 ) ;
#6032 = CARTESIAN_POINT ( 'NONE',  ( -3.492805317593278058, 46.55633131742322917, -10.50000000000000000 ) ) ;
#6033 = DIRECTION ( 'NONE',  ( 0.000000000000000000, 0.000000000000000000, 1.000000000000000000 ) ) ;
#6034 = ORIENTED_EDGE ( 'NONE', *, *, #13624, .T. ) ;
#6035 = ORIENTED_EDGE ( 'NONE', *, *, #6274, .T. ) ;
#6036 = CYLINDRICAL_SURFACE ( 'NONE', #11026, 100.0000000000000000 ) ;
#6037 = ORIENTED_EDGE ( 'NONE', *, *, #3161, .T. ) ;
#6038 = VECTOR ( 'NONE', #6294, 1000.000000000000000 ) ;
#6039 = EDGE_CURVE ( 'NONE', #2732, #6497, #5430, .T. ) ;
#6040 = DIRECTION ( 'NONE',  ( 1.000000000000000000, 0.000000000000000000, 0.000000000000000000 ) ) ;
#6041 = CIRCLE ( 'NONE', #7989, 107.0000000000000284 ) ;
#6042 = CARTESIAN_POINT ( 'NONE',  ( -12.39897948556635754, 61.76783392443436327, 16.00000000000000000 ) ) ;
#6043 = EDGE_CURVE ( 'NONE', #14940, #5135, #12016, .T. ) ;
#6044 = AXIS2_PLACEMENT_3D ( 'NONE', #5309, #14503, #4103 ) ;
#6045 = LINE ( 'NONE', #2572, #1321 ) ;
#6046 = LINE ( 'NONE', #10543, #10196 ) ;
#6047 = CARTESIAN_POINT ( 'NONE',  ( -49.00442420935969778, 30.80502811811250297, -10.50000000000000000 ) ) ;
#6048 = B_SPLINE_CURVE_WITH_KNOTS ( 'NONE', 3,
 ( #641, #11755, #14528, #5267, #4131, #13387, #10813, #2986, #7610, #10527, #127, #4767, #7382, #5041, #14027, #8243, #14298, #3908 ),
 .UNSPECIFIED., .F., .F.,
 ( 4, 2, 2, 2, 2, 2, 2, 2, 4 ),
 ( 0.001002887730653555286, 0.001856445934617267663, 0.002710004138580980257, 0.003563562342544692417, 0.004417120546508405445, 0.005270678750472117605, 0.006124236954435829765, 0.006977795158399542792, 0.007831353362363254952 ),
 .UNSPECIFIED. ) ;
#6049 = CARTESIAN_POINT ( 'NONE',  ( 0.2500000000000002220, 5.204748896376234922E-16, -4.250000000000000000 ) ) ;
#6050 = ORIENTED_EDGE ( 'NONE', *, *, #9543, .T. ) ;
#6051 = CYLINDRICAL_SURFACE ( 'NONE', #2418, 56.99999999999999289 ) ;
#6052 = AXIS2_PLACEMENT_3D ( 'NONE', #8796, #763, #13435 ) ;
#6053 = CIRCLE ( 'NONE', #9216, 17.00000000000000000 ) ;
#6054 = ORIENTED_EDGE ( 'NONE', *, *, #5139, .T. ) ;
#6055 = VECTOR ( 'NONE', #6298, 1000.000000000000000 ) ;
#6056 = VERTEX_POINT ( 'NONE', #1925 ) ;
#6057 = CARTESIAN_POINT ( 'NONE',  ( 0.000000000000000000, -4.618802153517023612, -3.433295621305388678 ) ) ;
#6058 = ORIENTED_EDGE ( 'NONE', *, *, #6282, .T. ) ;
#6059 = CARTESIAN_POINT ( 'NONE',  ( -56.43380494354004639, -12.86891638962099549, -8.000000000000000000 ) ) ;
#6060 = EDGE_CURVE ( 'NONE', #879, #5499, #5462, .T. ) ;
#6061 = ADVANCED_FACE ( 'NONE', ( #3082 ), #11124, .T. ) ;
#6062 = DIRECTION ( 'NONE',  ( 0.000000000000000000, 0.000000000000000000, 1.000000000000000000 ) ) ;
#6063 = AXIS2_PLACEMENT_3D ( 'NONE', #8722, #6589, #10100 ) ;
#6064 = CIRCLE ( 'NONE', #14576, 95.00000000000001421 ) ;
#6065 = CARTESIAN_POINT ( 'NONE',  ( -33.48561063518626923, 47.21331623427104063, -8.000000000000000000 ) ) ;
#6066 = DIRECTION ( 'NONE',  ( 1.000000000000000000, 0.000000000000000000, 0.000000000000000000 ) ) ;
#6067 = FACE_OUTER_BOUND ( 'NONE', #14436, .T. ) ;
#6068 = CIRCLE ( 'NONE', #14080, 50.00000000000000000 ) ;
#6069 = CARTESIAN_POINT ( 'NONE',  ( 33.47282819776613394, -39.30189486418255740, -8.000000000000000000 ) ) ;
#6070 = AXIS2_PLACEMENT_3D ( 'NONE', #12295, #8606, #14242 ) ;
#6071 = EDGE_LOOP ( 'NONE', ( #11836, #4164, #13029, #2550 ) ) ;
#6072 = DIRECTION ( 'NONE',  ( 0.000000000000000000, -1.000000000000000000, 1.287488025362403787E-15 ) ) ;
#6073 = ORIENTED_EDGE ( 'NONE', *, *, #14425, .F. ) ;
#6074 = VECTOR ( 'NONE', #2201, 1000.000000000000000 ) ;
#6075 = CARTESIAN_POINT ( 'NONE',  ( -7.829984960685305140, 106.7136390683879910, -20.00000000000000000 ) ) ;
#6076 = LINE ( 'NONE', #3823, #1773 ) ;
#6077 = AXIS2_PLACEMENT_3D ( 'NONE', #13737, #10450, #10307 ) ;
#6078 = CARTESIAN_POINT ( 'NONE',  ( 0.000000000000000000, 0.000000000000000000, 16.00000000000000000 ) ) ;
#6079 = AXIS2_PLACEMENT_3D ( 'NONE', #4610, #4762, #8316 ) ;
#6080 = CARTESIAN_POINT ( 'NONE',  ( 36.70371619500516402, 89.33979373934434420, 10.49999999999999822 ) ) ;
#6081 = AXIS2_PLACEMENT_3D ( 'NONE', #25, #9283, #13937 ) ;
#6082 = ORIENTED_EDGE ( 'NONE', *, *, #9654, .F. ) ;
#6083 = CARTESIAN_POINT ( 'NONE',  ( 2.449293598294700991E-16, -97.00000000000000000, 8.000000000000000000 ) ) ;
#6084 = ORIENTED_EDGE ( 'NONE', *, *, #1535, .T. ) ;
#6085 = APPLICATION_CONTEXT ( 'automotive_design' ) ;
#6086 = DIRECTION ( 'NONE',  ( 1.000000000000000000, 0.000000000000000000, 0.000000000000000000 ) ) ;
#6087 = DIRECTION ( 'NONE',  ( 0.000000000000000000, 0.000000000000000000, 1.000000000000000000 ) ) ;
#6088 = EDGE_CURVE ( 'NONE', #5824, #1620, #4013, .T. ) ;
#6089 = AXIS2_PLACEMENT_3D ( 'NONE', #6981, #8063, #13 ) ;
#6090 = CARTESIAN_POINT ( 'NONE',  ( -47.21331623427138879, -33.48561063518577896, -10.50000000000000000 ) ) ;
#6091 = ADVANCED_FACE ( 'NONE', ( #11279 ), #3226, .T. ) ;
#6092 = DIRECTION ( 'NONE',  ( -1.000000000000000000, 0.000000000000000000, 0.000000000000000000 ) ) ;
#6093 = EDGE_LOOP ( 'NONE', ( #14197, #7471, #6272, #5785, #12288 ) ) ;
#6094 = AXIS2_PLACEMENT_3D ( 'NONE', #11056, #4706, #7108 ) ;
#6095 = EDGE_LOOP ( 'NONE', ( #4474, #10084, #7049, #4567 ) ) ;
#6096 = DIRECTION ( 'NONE',  ( 1.000000000000000000, 0.000000000000000000, 0.000000000000000000 ) ) ;
#6097 = DIRECTION ( 'NONE',  ( 1.000000000000000000, 0.000000000000000000, 0.000000000000000000 ) ) ;
#6098 = CARTESIAN_POINT ( 'NONE',  ( 68.09867107462983427, 68.49330278050145182, 10.49999999999999822 ) ) ;
#6099 = EDGE_CURVE ( 'NONE', #11061, #9394, #14917, .T. ) ;
#6100 =( GEOMETRIC_REPRESENTATION_CONTEXT ( 3 ) GLOBAL_UNCERTAINTY_ASSIGNED_CONTEXT ( ( #7728 ) ) GLOBAL_UNIT_ASSIGNED_CONTEXT ( ( #7505, #3889, #460 ) ) REPRESENTATION_CONTEXT ( 'NONE', 'WORKASPACE' ) );
#6101 = ORIENTED_EDGE ( 'NONE', *, *, #6734, .T. ) ;
#6102 = VERTEX_POINT ( 'NONE', #14770 ) ;
#6103 = AXIS2_PLACEMENT_3D ( 'NONE', #14451, #4057, #13304 ) ;
#6104 = CARTESIAN_POINT ( 'NONE',  ( 68.58935777509475429, -68.58935777509547904, -8.000000000000000000 ) ) ;
#6105 = ORIENTED_EDGE ( 'NONE', *, *, #1890, .T. ) ;
#6106 = CARTESIAN_POINT ( 'NONE',  ( 0.000000000000000000, 0.000000000000000000, -10.50000000000000000 ) ) ;
#6107 = EDGE_CURVE ( 'NONE', #14931, #9719, #1816, .T. ) ;
#6108 = CARTESIAN_POINT ( 'NONE',  ( 11.62509980388830222, 61.91833518448028428, -17.84018927347701577 ) ) ;
#6109 = ADVANCED_FACE ( 'NONE', ( #10053 ), #10200, .F. ) ;
#6110 = DIRECTION ( 'NONE',  ( 0.000000000000000000, 0.000000000000000000, -1.000000000000000000 ) ) ;
#6111 = DIRECTION ( 'NONE',  ( 1.000000000000000000, 0.000000000000000000, 0.000000000000000000 ) ) ;
#6112 = ORIENTED_EDGE ( 'NONE', *, *, #2272, .F. ) ;
#6113 = ORIENTED_EDGE ( 'NONE', *, *, #559, .T. ) ;
#6114 = AXIS2_PLACEMENT_3D ( 'NONE', #7230, #8310, #7311 ) ;
#6115 = ORIENTED_EDGE ( 'NONE', *, *, #8514, .F. ) ;
#6116 = CARTESIAN_POINT ( 'NONE',  ( 0.000000000000000000, 0.000000000000000000, -25.50000000000000355 ) ) ;
#6117 = CARTESIAN_POINT ( 'NONE',  ( -19.68583958711381854, -30.74264578624812927, -25.50000000000000355 ) ) ;
#6118 = CARTESIAN_POINT ( 'NONE',  ( -45.89934640057513349, 26.50000000000019540, -10.50000000000000000 ) ) ;
#6119 = ORIENTED_EDGE ( 'NONE', *, *, #5559, .T. ) ;
#6120 = ORIENTED_EDGE ( 'NONE', *, *, #8414, .T. ) ;
#6121 = DIRECTION ( 'NONE',  ( -1.000000000000000000, 0.000000000000000000, 0.000000000000000000 ) ) ;
#6122 = EDGE_LOOP ( 'NONE', ( #5727, #14745, #13789, #6073, #11543 ) ) ;
#6123 = DIRECTION ( 'NONE',  ( -1.000000000000000000, 0.000000000000000000, 0.000000000000000000 ) ) ;
#6124 = DIRECTION ( 'NONE',  ( -0.000000000000000000, -0.000000000000000000, 1.000000000000000000 ) ) ;
#6125 = DIRECTION ( 'NONE',  ( 0.000000000000000000, 0.000000000000000000, 1.000000000000000000 ) ) ;
#6126 = AXIS2_PLACEMENT_3D ( 'NONE', #6948, #12582, #2173 ) ;
#6127 = CARTESIAN_POINT ( 'NONE',  ( 56.43380494353997534, 12.86891638962136319, -8.000000000000000000 ) ) ;
#6128 = CARTESIAN_POINT ( 'NONE',  ( -33.48561063518626923, 47.21331623427104063, 8.000000000000000000 ) ) ;
#6129 = ORIENTED_EDGE ( 'NONE', *, *, #12754, .T. ) ;
#6130 = CARTESIAN_POINT ( 'NONE',  ( 0.000000000000000000, 0.000000000000000000, 10.50000000000000000 ) ) ;
#6131 = AXIS2_PLACEMENT_3D ( 'NONE', #9670, #14401, #2713 ) ;
#6132 = EDGE_LOOP ( 'NONE', ( #5729, #8329, #951, #2668, #5696 ) ) ;
#6133 = ORIENTED_EDGE ( 'NONE', *, *, #7648, .F. ) ;
#6134 = DIRECTION ( 'NONE',  ( 0.000000000000000000, 0.000000000000000000, -1.000000000000000000 ) ) ;
#6135 = ORIENTED_EDGE ( 'NONE', *, *, #13259, .T. ) ;
#6136 = VECTOR ( 'NONE', #7381, 1000.000000000000000 ) ;
#6137 = CYLINDRICAL_SURFACE ( 'NONE', #14169, 0.5000000000000004441 ) ;
#6138 = VERTEX_POINT ( 'NONE', #7923 ) ;
#6139 = DIRECTION ( 'NONE',  ( 1.000000000000000000, 0.000000000000000000, 0.000000000000000000 ) ) ;
#6140 = DIRECTION ( 'NONE',  ( -0.000000000000000000, -0.000000000000000000, 1.000000000000000000 ) ) ;
#6141 = DIRECTION ( 'NONE',  ( -0.000000000000000000, -0.000000000000000000, -1.000000000000000000 ) ) ;
#6142 = DIRECTION ( 'NONE',  ( 0.000000000000000000, 0.000000000000000000, 1.000000000000000000 ) ) ;
#6143 = FACE_OUTER_BOUND ( 'NONE', #3431, .T. ) ;
#6144 = ORIENTED_EDGE ( 'NONE', *, *, #1944, .T. ) ;
#6145 = AXIS2_PLACEMENT_3D ( 'NONE', #13391, #4439, #12265 ) ;
#6146 = CONICAL_SURFACE ( 'NONE', #2284, 2.055000000000000160, 0.7853981633974479459 ) ;
#6147 = AXIS2_PLACEMENT_3D ( 'NONE', #9858, #4101, #8569 ) ;
#6148 = CARTESIAN_POINT ( 'NONE',  ( 68.58935777509523746, 68.58935777509499587, -13.00000000000000178 ) ) ;
#6149 = AXIS2_PLACEMENT_3D ( 'NONE', #9726, #8594, #14455 ) ;
#6150 = EDGE_LOOP ( 'NONE', ( #568, #6349, #9056, #12004, #13815, #2484, #3704, #12411 ) ) ;
#6151 = EDGE_CURVE ( 'NONE', #13119, #2051, #7144, .T. ) ;
#6152 = ADVANCED_FACE ( 'NONE', ( #5351 ), #1862, .F. ) ;
#6153 = ADVANCED_FACE ( 'NONE', ( #8834 ), #13476, .F. ) ;
#6154 = CARTESIAN_POINT ( 'NONE',  ( 2.500000000000002220, 1.178949249685208533, -2.042000000000002036 ) ) ;
#6155 = CARTESIAN_POINT ( 'NONE',  ( -41.54772703543551415, -32.26435573746212526, 10.49999999999999822 ) ) ;
#6156 = DIRECTION ( 'NONE',  ( 1.000000000000000000, 0.000000000000000000, -0.000000000000000000 ) ) ;
#6157 = FACE_OUTER_BOUND ( 'NONE', #657, .T. ) ;
#6158 = EDGE_LOOP ( 'NONE', ( #8298, #9643, #7961, #4203 ) ) ;
#6159 = VERTEX_POINT ( 'NONE', #12789 ) ;
#6160 = CIRCLE ( 'NONE', #14667, 60.50000000000000000 ) ;
#6161 = CIRCLE ( 'NONE', #13443, 2.041999999999999815 ) ;
#6162 = CARTESIAN_POINT ( 'NONE',  ( 12.50000000000000000, 100.2235002382176248, 15.33678752976415716 ) ) ;
#6163 = ORIENTED_EDGE ( 'NONE', *, *, #619, .F. ) ;
#6164 = DIRECTION ( 'NONE',  ( 0.000000000000000000, 0.000000000000000000, -1.000000000000000000 ) ) ;
#6165 = LINE ( 'NONE', #14294, #4669 ) ;
#6166 = CARTESIAN_POINT ( 'NONE',  ( -68.01302780753309207, 65.64523757230344359, -13.00000000000000178 ) ) ;
#6167 = CARTESIAN_POINT ( 'NONE',  ( -20.00000000000000000, 2.449293598294706513E-15, -45.50000000000000000 ) ) ;
#6168 = LINE ( 'NONE', #1776, #10716 ) ;
#6169 = AXIS2_PLACEMENT_3D ( 'NONE', #2637, #1506, #6121 ) ;
#6170 = ORIENTED_EDGE ( 'NONE', *, *, #7648, .T. ) ;
#6171 = VECTOR ( 'NONE', #14936, 1000.000000000000000 ) ;
#6172 = DIRECTION ( 'NONE',  ( 0.000000000000000000, 0.000000000000000000, -1.000000000000000000 ) ) ;
#6173 = CYLINDRICAL_SURFACE ( 'NONE', #11290, 22.00000000000001421 ) ;
#6174 = VECTOR ( 'NONE', #6977, 1000.000000000000000 ) ;
#6175 = DIRECTION ( 'NONE',  ( 0.000000000000000000, 0.4999999999999995559, -0.8660254037844389297 ) ) ;
#6176 = ADVANCED_FACE ( 'NONE', ( #10281 ), #9285, .T. ) ;
#6177 = ORIENTED_EDGE ( 'NONE', *, *, #3021, .T. ) ;
#6178 = DIRECTION ( 'NONE',  ( -0.000000000000000000, -0.000000000000000000, 1.000000000000000000 ) ) ;
#6179 = AXIS2_PLACEMENT_3D ( 'NONE', #698, #1982, #11252 ) ;
#6180 = VERTEX_POINT ( 'NONE', #12938 ) ;
#6181 = CARTESIAN_POINT ( 'NONE',  ( -18.52941176470586981, 60.21346111671361001, -16.00000000000000000 ) ) ;
#6182 = TOROIDAL_SURFACE ( 'NONE', #8132, 5.384454397937118664, 0.5155456020628804703 ) ;
#6183 = CARTESIAN_POINT ( 'NONE',  ( 10.87743925404099876, 62.05426862177564118, -18.69798886497097712 ) ) ;
#6184 = CARTESIAN_POINT ( 'NONE',  ( -0.1756481739660510633, 4.720212674038980261, -3.469390959564067067 ) ) ;
#6185 = SURFACE_STYLE_USAGE ( .BOTH. , #8398 ) ;
#6186 = CARTESIAN_POINT ( 'NONE',  ( 32.26435573746228158, -42.04772703543541468, -13.00000000000000178 ) ) ;
#6187 = ORIENTED_EDGE ( 'NONE', *, *, #6107, .T. ) ;
#6188 = LINE ( 'NONE', #4997, #3020 ) ;
#6189 = DIRECTION ( 'NONE',  ( 1.000000000000000000, 0.000000000000000000, 0.000000000000000000 ) ) ;
#6190 = AXIS2_PLACEMENT_3D ( 'NONE', #14957, #3487, #10389 ) ;
#6191 = CARTESIAN_POINT ( 'NONE',  ( 12.50000000000000000, 100.2235002382176248, -15.00000000000000000 ) ) ;
#6192 = ORIENTED_EDGE ( 'NONE', *, *, #6798, .F. ) ;
#6193 = EDGE_CURVE ( 'NONE', #7026, #14497, #13713, .T. ) ;
#6194 = ADVANCED_FACE ( 'NONE', ( #3369 ), #9139, .T. ) ;
#6195 = VERTEX_POINT ( 'NONE', #10503 ) ;
#6196 = DIRECTION ( 'NONE',  ( 1.000000000000000000, 0.000000000000000000, 0.000000000000000000 ) ) ;
#6197 = ORIENTED_EDGE ( 'NONE', *, *, #12432, .F. ) ;
#6198 =( REPRESENTATION_RELATIONSHIP ('NONE','NONE', #12187, #12767 ) REPRESENTATION_RELATIONSHIP_WITH_TRANSFORMATION ( #9345 )SHAPE_REPRESENTATION_RELATIONSHIP( ) );
#6199 = AXIS2_PLACEMENT_3D ( 'NONE', #14378, #3985, #8600 ) ;
#6200 = DIRECTION ( 'NONE',  ( -0.000000000000000000, -0.000000000000000000, 1.000000000000000000 ) ) ;
#6201 = CARTESIAN_POINT ( 'NONE',  ( 14.00000000000000000, 1.714505518806294638E-15, 14.49999999999999822 ) ) ;
#6202 = EDGE_CURVE ( 'NONE', #11991, #7285, #486, .T. ) ;
#6203 = ORIENTED_EDGE ( 'NONE', *, *, #1164, .F. ) ;
#6204 = CARTESIAN_POINT ( 'NONE',  ( 12.94095225512611869, -48.29629131445339851, 8.000000000000000000 ) ) ;
#6205 = CARTESIAN_POINT ( 'NONE',  ( 1.674280531759324342, 99.48933418828643482, 8.000000000000000000 ) ) ;
#6206 = ORIENTED_EDGE ( 'NONE', *, *, #13962, .T. ) ;
#6207 = DIRECTION ( 'NONE',  ( 1.000000000000000000, 0.000000000000000000, 0.000000000000000000 ) ) ;
#6208 = CIRCLE ( 'NONE', #5258, 3.000000000000002665 ) ;
#6209 = ORIENTED_EDGE ( 'NONE', *, *, #7070, .F. ) ;
#6210 = EDGE_CURVE ( 'NONE', #11466, #1453, #11158, .T. ) ;
#6211 = ORIENTED_EDGE ( 'NONE', *, *, #8437, .F. ) ;
#6212 = DIRECTION ( 'NONE',  ( 0.000000000000000000, 0.000000000000000000, 1.000000000000000000 ) ) ;
#6213 = DIRECTION ( 'NONE',  ( -1.000000000000000000, 0.000000000000000000, 0.000000000000000000 ) ) ;
#6214 = DIRECTION ( 'NONE',  ( -1.000000000000000000, 0.000000000000000000, 0.000000000000000000 ) ) ;
#6215 = LINE ( 'NONE', #14276, #9954 ) ;
#6216 = DIRECTION ( 'NONE',  ( 1.000000000000000000, 0.000000000000000000, 0.000000000000000000 ) ) ;
#6217 = CARTESIAN_POINT ( 'NONE',  ( -53.26842454702436669, -11.55014193876159645, -8.000000000000000000 ) ) ;
#6218 = ORIENTED_EDGE ( 'NONE', *, *, #4652, .T. ) ;
#6219 = EDGE_LOOP ( 'NONE', ( #7937, #14520, #3359, #1904, #1295, #7931 ) ) ;
#6220 = DIRECTION ( 'NONE',  ( 0.000000000000000000, 0.000000000000000000, -1.000000000000000000 ) ) ;
#6221 = DIRECTION ( 'NONE',  ( -0.000000000000000000, -0.000000000000000000, 1.000000000000000000 ) ) ;
#6222 = ORIENTED_EDGE ( 'NONE', *, *, #619, .T. ) ;
#6223 = DIRECTION ( 'NONE',  ( -0.000000000000000000, -0.000000000000000000, 1.000000000000000000 ) ) ;
#6224 = ORIENTED_EDGE ( 'NONE', *, *, #5312, .T. ) ;
#6225 = DIRECTION ( 'NONE',  ( -0.000000000000000000, -0.000000000000000000, 1.000000000000000000 ) ) ;
#6226 = ORIENTED_EDGE ( 'NONE', *, *, #7724, .T. ) ;
#6227 = CARTESIAN_POINT ( 'NONE',  ( 12.39897948556635754, 100.2360479454198696, 16.00000000000000000 ) ) ;
#6228 = EDGE_LOOP ( 'NONE', ( #6678, #3740, #4597, #7694, #12186, #9214, #10672, #5641, #6120, #5407 ) ) ;
#6229 = DIRECTION ( 'NONE',  ( -1.000000000000000000, 0.000000000000000000, 0.000000000000000000 ) ) ;
#6230 = EDGE_CURVE ( 'NONE', #4760, #2764, #5333, .T. ) ;
#6231 = CARTESIAN_POINT ( 'NONE',  ( -29.70588235294118107, 96.53269163155674448, -10.99999999999999645 ) ) ;
#6232 = EDGE_CURVE ( 'NONE', #14105, #7249, #2452, .T. ) ;
#6233 = CARTESIAN_POINT ( 'NONE',  ( -32.45630819848046400, 101.9391205390361534, -14.06872601623944519 ) ) ;
#6234 = CARTESIAN_POINT ( 'NONE',  ( 5.200000000000006395, 0.000000000000000000, -2.699999999999972644 ) ) ;
#6235 = FACE_OUTER_BOUND ( 'NONE', #7787, .T. ) ;
#6236 = ORIENTED_EDGE ( 'NONE', *, *, #125, .T. ) ;
#6237 = FACE_OUTER_BOUND ( 'NONE', #3467, .T. ) ;
#6238 = ADVANCED_FACE ( 'NONE', ( #10356 ), #7071, .T. ) ;
#6239 = DIRECTION ( 'NONE',  ( 1.000000000000000000, 0.000000000000000000, 0.000000000000000000 ) ) ;
#6240 = CARTESIAN_POINT ( 'NONE',  ( -4.999999999999996447, 85.00000000000000000, 31.00000000000000000 ) ) ;
#6241 = EDGE_LOOP ( 'NONE', ( #5437, #6630, #327, #4299 ) ) ;
#6242 = EDGE_CURVE ( 'NONE', #13650, #12160, #5502, .T. ) ;
#6243 = PLANE ( 'NONE',  #9476 ) ;
#6244 = ORIENTED_EDGE ( 'NONE', *, *, #444, .F. ) ;
#6245 = CARTESIAN_POINT ( 'NONE',  ( -92.38795325112907619, -38.26834323650804492, -8.000000000000000000 ) ) ;
#6246 = ADVANCED_FACE ( 'NONE', ( #9210 ), #2238, .T. ) ;
#6247 = DIRECTION ( 'NONE',  ( 0.000000000000000000, 0.000000000000000000, 1.000000000000000000 ) ) ;
#6248 = LINE ( 'NONE', #1642, #820 ) ;
#6249 = DIRECTION ( 'NONE',  ( 1.000000000000000000, 0.000000000000000000, 0.000000000000000000 ) ) ;
#6250 = DIRECTION ( 'NONE',  ( 1.000000000000000000, 0.000000000000000000, 0.000000000000000000 ) ) ;
#6251 = AXIS2_PLACEMENT_3D ( 'NONE', #2205, #11627, #1000 ) ;
#6252 = ORIENTED_EDGE ( 'NONE', *, *, #7073, .T. ) ;
#6253 = DIRECTION ( 'NONE',  ( -1.000000000000000000, 0.000000000000000000, 0.000000000000000000 ) ) ;
#6254 = DIRECTION ( 'NONE',  ( -0.000000000000000000, -0.000000000000000000, -1.000000000000000000 ) ) ;
#6255 = CARTESIAN_POINT ( 'NONE',  ( 22.33583958711425055, -30.74264578624780597, -25.50000000000000355 ) ) ;
#6256 = ORIENTED_EDGE ( 'NONE', *, *, #3345, .T. ) ;
#6257 = ORIENTED_EDGE ( 'NONE', *, *, #3663, .T. ) ;
#6258 = DIRECTION ( 'NONE',  ( -1.000000000000000000, 0.000000000000000000, 0.000000000000000000 ) ) ;
#6259 = EDGE_LOOP ( 'NONE', ( #14986, #14402, #3865, #2699 ) ) ;
#6260 = FACE_OUTER_BOUND ( 'NONE', #6095, .T. ) ;
#6261 = CARTESIAN_POINT ( 'NONE',  ( -15.88467684210512942, 49.11971303961693280, -13.00000000000000178 ) ) ;
#6262 = EDGE_CURVE ( 'NONE', #2264, #1542, #6992, .T. ) ;
#6264 = ORIENTED_EDGE ( 'NONE', *, *, #8414, .F. ) ;
#6263 = EDGE_CURVE ( 'NONE', #2119, #1055, #14305, .T. ) ;
#6265 = VERTEX_POINT ( 'NONE', #11516 ) ;
#6266 = DIRECTION ( 'NONE',  ( 1.000000000000000000, 0.000000000000000000, 0.000000000000000000 ) ) ;
#6267 = DIRECTION ( 'NONE',  ( -1.000000000000000000, 0.000000000000000000, -0.000000000000000000 ) ) ;
#6268 = EDGE_CURVE ( 'NONE', #197, #12197, #5092, .T. ) ;
#6269 = ORIENTED_EDGE ( 'NONE', *, *, #3139, .F. ) ;
#6270 = DIRECTION ( 'NONE',  ( 1.000000000000000000, 0.000000000000000000, 0.000000000000000000 ) ) ;
#6271 = ORIENTED_EDGE ( 'NONE', *, *, #1752, .F. ) ;
#6272 = ORIENTED_EDGE ( 'NONE', *, *, #10515, .T. ) ;
#6273 = CARTESIAN_POINT ( 'NONE',  ( -30.33882973767906321, 96.33581297378611907, 13.50942224097978617 ) ) ;
#6274 = EDGE_CURVE ( 'NONE', #8032, #1839, #12622, .T. ) ;
#6275 = CIRCLE ( 'NONE', #9668, 22.00000000000000000 ) ;
#6276 = CARTESIAN_POINT ( 'NONE',  ( 32.10455955028198360, 102.0624585623582306, -13.51511155787191854 ) ) ;
#6277 = CARTESIAN_POINT ( 'NONE',  ( -13.21740939043329099, 51.19406879332069593, -13.00000000000000178 ) ) ;
#6278 = CARTESIAN_POINT ( 'NONE',  ( -26.49999999999971578, -45.89934640057541060, -10.50000000000000000 ) ) ;
#6279 = CARTESIAN_POINT ( 'NONE',  ( 42.00000000000000711, 81.24038404635960831, 26.00000000000000000 ) ) ;
#6280 = AXIS2_PLACEMENT_3D ( 'NONE', #5458, #5233, #680 ) ;
#6281 = DIRECTION ( 'NONE',  ( 0.000000000000000000, 0.000000000000000000, 1.000000000000000000 ) ) ;
#6282 = EDGE_CURVE ( 'NONE', #944, #7811, #3678, .T. ) ;
#6283 = VERTEX_POINT ( 'NONE', #5037 ) ;
#6284 = AXIS2_PLACEMENT_3D ( 'NONE', #7994, #11592, #6930 ) ;
#6285 = CYLINDRICAL_SURFACE ( 'NONE', #13848, 56.99999999999999289 ) ;
#6286 = ORIENTED_EDGE ( 'NONE', *, *, #14274, .F. ) ;
#6287 = LINE ( 'NONE', #11097, #14234 ) ;
#6288 = LINE ( 'NONE', #464, #14139 ) ;
#6289 = ORIENTED_EDGE ( 'NONE', *, *, #8284, .T. ) ;
#6290 = CARTESIAN_POINT ( 'NONE',  ( -32.26435573746199736, 42.04772703543562073, 8.000000000000000000 ) ) ;
#6291 = CIRCLE ( 'NONE', #9690, 3.000000000000002665 ) ;
#6292 = CARTESIAN_POINT ( 'NONE',  ( 55.00000000000000711, 0.000000000000000000, 0.000000000000000000 ) ) ;
#6293 = ORIENTED_EDGE ( 'NONE', *, *, #5967, .F. ) ;
#6294 = DIRECTION ( 'NONE',  ( 0.000000000000000000, 0.000000000000000000, 1.000000000000000000 ) ) ;
#6295 = AXIS2_PLACEMENT_3D ( 'NONE', #10784, #229, #12919 ) ;
#6296 = ORIENTED_EDGE ( 'NONE', *, *, #3604, .F. ) ;
#6297 = VECTOR ( 'NONE', #6514, 1000.000000000000000 ) ;
#6298 = DIRECTION ( 'NONE',  ( 0.000000000000000000, 0.000000000000000000, 1.000000000000000000 ) ) ;
#6299 = LINE ( 'NONE', #9803, #6841 ) ;
#6300 = CARTESIAN_POINT ( 'NONE',  ( -34.09969740539978034, 101.2725728942521215, -15.50446122302711949 ) ) ;
#6301 = CARTESIAN_POINT ( 'NONE',  ( 53.63365512954693770, -9.714003807513686084, -8.000000000000000000 ) ) ;
#6302 = DIRECTION ( 'NONE',  ( -1.000000000000000000, 0.000000000000000000, 0.000000000000000000 ) ) ;
#6303 = AXIS2_PLACEMENT_3D ( 'NONE', #11839, #8553, #11919 ) ;
#6304 = EDGE_LOOP ( 'NONE', ( #7195, #1679, #12345, #5126, #3107 ) ) ;
#6305 = FACE_OUTER_BOUND ( 'NONE', #12311, .T. ) ;
#6306 = AXIS2_PLACEMENT_3D ( 'NONE', #7940, #11010, #2172 ) ;
#6307 = CYLINDRICAL_SURFACE ( 'NONE', #11765, 3.000000000000002665 ) ;
#6308 = AXIS2_PLACEMENT_3D ( 'NONE', #7567, #14264, #376 ) ;
#6309 = CARTESIAN_POINT ( 'NONE',  ( 0.000000000000000000, 0.000000000000000000, -4.694516984716113228 ) ) ;
#6310 = EDGE_CURVE ( 'NONE', #604, #5762, #1690, .T. ) ;
#6311 = EDGE_LOOP ( 'NONE', ( #10914, #7549, #8455, #4624 ) ) ;
#6312 = PRODUCT ( 'wheel hub', 'wheel hub', '', ( #9272 ) ) ;
#6313 = ORIENTED_EDGE ( 'NONE', *, *, #2179, .F. ) ;
#6314 = CARTESIAN_POINT ( 'NONE',  ( 0.000000000000000000, 0.000000000000000000, -10.50000000000000000 ) ) ;
#6315 = EDGE_LOOP ( 'NONE', ( #6935, #802, #8505, #7360 ) ) ;
#6316 = CIRCLE ( 'NONE', #7047, 2.649999999999987477 ) ;
#6317 = CARTESIAN_POINT ( 'NONE',  ( 1.674280531759324342, 99.48933418828643482, -8.000000000000000000 ) ) ;
#6318 = DIRECTION ( 'NONE',  ( 0.000000000000000000, 0.000000000000000000, -1.000000000000000000 ) ) ;
#6319 = FACE_OUTER_BOUND ( 'NONE', #6219, .T. ) ;
#6320 = DIRECTION ( 'NONE',  ( 0.000000000000000000, 0.000000000000000000, 1.000000000000000000 ) ) ;
#6321 = CARTESIAN_POINT ( 'NONE',  ( 36.14014761921571051, 11.74264578624840993, 19.49999999999999645 ) ) ;
#6322 = CARTESIAN_POINT ( 'NONE',  ( 0.000000000000000000, 0.000000000000000000, -10.50000000000000000 ) ) ;
#6323 = VERTEX_POINT ( 'NONE', #3976 ) ;
#6324 = ORIENTED_EDGE ( 'NONE', *, *, #10135, .F. ) ;
#6325 = DIRECTION ( 'NONE',  ( 0.000000000000000000, 1.000000000000000000, 0.000000000000000000 ) ) ;
#6326 = DIRECTION ( 'NONE',  ( 0.000000000000000000, 0.000000000000000000, 1.000000000000000000 ) ) ;
#6327 = AXIS2_PLACEMENT_3D ( 'NONE', #13846, #9347, #9489 ) ;
#6328 = EDGE_CURVE ( 'NONE', #9063, #11311, #9450, .T. ) ;
#6329 = CYLINDRICAL_SURFACE ( 'NONE', #3244, 63.00000000000000000 ) ;
#6330 = ADVANCED_FACE ( 'NONE', ( #8520 ), #9644, .F. ) ;
#6332 = ORIENTED_EDGE ( 'NONE', *, *, #1110, .T. ) ;
#6331 = ADVANCED_FACE ( 'NONE', ( #13087 ), #1547, .F. ) ;
#6333 = AXIS2_PLACEMENT_3D ( 'NONE', #656, #9980, #11352 ) ;
#6334 = VERTEX_POINT ( 'NONE', #12035 ) ;
#6335 = DIRECTION ( 'NONE',  ( -1.000000000000000000, 0.000000000000000000, 0.000000000000000000 ) ) ;
#6336 = ADVANCED_FACE ( 'NONE', ( #8590, #4970 ), #332, .T. ) ;
#6337 = ORIENTED_EDGE ( 'NONE', *, *, #5913, .F. ) ;
#6338 = DIRECTION ( 'NONE',  ( -1.000000000000000000, 0.000000000000000000, 0.000000000000000000 ) ) ;
#6339 = AXIS2_PLACEMENT_3D ( 'NONE', #12428, #7856, #14481 ) ;
#6340 = DIRECTION ( 'NONE',  ( 0.000000000000000000, 0.000000000000000000, 1.000000000000000000 ) ) ;
#6341 = CARTESIAN_POINT ( 'NONE',  ( 6.526309611002977462, 49.57224306869046870, -8.000000000000000000 ) ) ;
#6342 = DIRECTION ( 'NONE',  ( -1.000000000000000000, 0.000000000000000000, -0.000000000000000000 ) ) ;
#6343 = VECTOR ( 'NONE', #637, 1000.000000000000000 ) ;
#6344 = VERTEX_POINT ( 'NONE', #4893 ) ;
#6345 = DIRECTION ( 'NONE',  ( 0.000000000000000000, 0.000000000000000000, 1.000000000000000000 ) ) ;
#6346 = ORIENTED_EDGE ( 'NONE', *, *, #4329, .T. ) ;
#6347 = CIRCLE ( 'NONE', #4757, 60.50000000000000000 ) ;
#6348 = CIRCLE ( 'NONE', #2488, 0.5000000000000004441 ) ;
#6349 = ORIENTED_EDGE ( 'NONE', *, *, #9257, .T. ) ;
#6350 = FACE_OUTER_BOUND ( 'NONE', #7756, .T. ) ;
#6351 = ADVANCED_FACE ( 'NONE', ( #14293 ), #9802, .T. ) ;
#6352 = CARTESIAN_POINT ( 'NONE',  ( 0.000000000000000000, 0.000000000000000000, -45.50000000000000000 ) ) ;
#6353 = CIRCLE ( 'NONE', #14875, 2.649999999999985700 ) ;
#6354 = EDGE_CURVE ( 'NONE', #7414, #7196, #3647, .T. ) ;
#6355 = CARTESIAN_POINT ( 'NONE',  ( -49.00442420935969778, 30.80502811811250297, -10.50000000000000000 ) ) ;
#6356 = CYLINDRICAL_SURFACE ( 'NONE', #9969, 50.00000000000000000 ) ;
#6357 = DIRECTION ( 'NONE',  ( 0.000000000000000000, 0.000000000000000000, 1.000000000000000000 ) ) ;
#6358 = DIRECTION ( 'NONE',  ( 0.000000000000000000, 0.000000000000000000, -1.000000000000000000 ) ) ;
#6359 = CIRCLE ( 'NONE', #1303, 0.2500000000000002220 ) ;
#6360 = ORIENTED_EDGE ( 'NONE', *, *, #9126, .T. ) ;
#6361 = CARTESIAN_POINT ( 'NONE',  ( 0.000000000000000000, 0.000000000000000000, 16.00000000000000000 ) ) ;
#6362 = DIRECTION ( 'NONE',  ( 1.000000000000000000, 0.000000000000000000, 0.000000000000000000 ) ) ;
#6363 = DIRECTION ( 'NONE',  ( 0.000000000000000000, 0.000000000000000000, 1.000000000000000000 ) ) ;
#6364 = DIRECTION ( 'NONE',  ( 0.000000000000000000, 0.000000000000000000, 1.000000000000000000 ) ) ;
#6365 = AXIS2_PLACEMENT_3D ( 'NONE', #8684, #13322, #11058 ) ;
#6366 = EDGE_LOOP ( 'NONE', ( #5675, #989, #12701, #6503 ) ) ;
#6367 = CYLINDRICAL_SURFACE ( 'NONE', #6179, 63.00000000000000000 ) ;
#6368 = EDGE_LOOP ( 'NONE', ( #2724, #10694, #984, #8376, #12732, #2349, #2041, #11802, #13467 ) ) ;
#6369 = EDGE_CURVE ( 'NONE', #1906, #8030, #7378, .T. ) ;
#6370 = FACE_BOUND ( 'NONE', #4277, .T. ) ;
#6371 = AXIS2_PLACEMENT_3D ( 'NONE', #7707, #9992, #5287 ) ;
#6372 = EDGE_CURVE ( 'NONE', #14250, #14615, #14229, .T. ) ;
#6373 = ORIENTED_EDGE ( 'NONE', *, *, #11619, .T. ) ;
#6374 = CARTESIAN_POINT ( 'NONE',  ( -51.45950017607691507, 4.121772567811807342, -8.000000000000000000 ) ) ;
#6375 = ORIENTED_EDGE ( 'NONE', *, *, #9672, .T. ) ;
#6376 = CARTESIAN_POINT ( 'NONE',  ( 0.000000000000000000, 0.000000000000000000, 13.00000000000000178 ) ) ;
#6377 = CARTESIAN_POINT ( 'NONE',  ( -51.53979475227126983, -13.35619814848815601, 10.49999999999999822 ) ) ;
#6378 = CYLINDRICAL_SURFACE ( 'NONE', #2734, 100.0000000000000000 ) ;
#6379 = CIRCLE ( 'NONE', #14893, 59.50000000000000000 ) ;
#6380 = VECTOR ( 'NONE', #10067, 1000.000000000000000 ) ;
#6381 = CIRCLE ( 'NONE', #14659, 2.500000000000000888 ) ;
#6382 = CARTESIAN_POINT ( 'NONE',  ( -34.93865171984689511, 100.8681255216228578, -15.83776386865433672 ) ) ;
#6383 = DIRECTION ( 'NONE',  ( 0.000000000000000000, 0.000000000000000000, 1.000000000000000000 ) ) ;
#6384 = EDGE_CURVE ( 'NONE', #11004, #1282, #4381, .T. ) ;
#6385 = CARTESIAN_POINT ( 'NONE',  ( -37.21932736666205699, 89.12622059913296368, 10.49999999999999822 ) ) ;
#6386 = EDGE_LOOP ( 'NONE', ( #12300, #6360, #5020, #7840, #4817, #5397, #9607, #1668, #12715 ) ) ;
#6387 = DIRECTION ( 'NONE',  ( 1.000000000000000000, 0.000000000000000000, 0.000000000000000000 ) ) ;
#6388 = FACE_OUTER_BOUND ( 'NONE', #3807, .T. ) ;
#6389 = UNCERTAINTY_MEASURE_WITH_UNIT (LENGTH_MEASURE( 1.000000000000000082E-05 ), #675, 'distance_accuracy_value', 'NONE');
#6390 = CARTESIAN_POINT ( 'NONE',  ( 3.999999999999998224, 2.472263674411416812, -3.687027874309863229 ) ) ;
#6391 = AXIS2_PLACEMENT_3D ( 'NONE', #10231, #1278, #12814 ) ;
#6392 = CIRCLE ( 'NONE', #7376, 22.00000000000000000 ) ;
#6393 = ORIENTED_EDGE ( 'NONE', *, *, #3854, .T. ) ;
#6394 = DIRECTION ( 'NONE',  ( -0.000000000000000000, -0.000000000000000000, 1.000000000000000000 ) ) ;
#6395 = ORIENTED_EDGE ( 'NONE', *, *, #8159, .T. ) ;
#6396 = DIRECTION ( 'NONE',  ( 0.000000000000000000, 1.000000000000000000, -0.000000000000000000 ) ) ;
#6397 = CARTESIAN_POINT ( 'NONE',  ( -36.52608637591512775, 92.55687898036946137, -13.00000000000000178 ) ) ;
#6398 = ORIENTED_EDGE ( 'NONE', *, *, #8604, .F. ) ;
#6399 = AXIS2_PLACEMENT_3D ( 'NONE', #6988, #8069, #14992 ) ;
#6400 = PLANE ( 'NONE',  #1239 ) ;
#6401 = DIRECTION ( 'NONE',  ( -1.000000000000000000, 0.000000000000000000, 0.000000000000000000 ) ) ;
#6402 = DIRECTION ( 'NONE',  ( -1.000000000000000000, 0.000000000000000000, 6.123233995736766036E-17 ) ) ;
#6403 = ORIENTED_EDGE ( 'NONE', *, *, #8969, .T. ) ;
#6404 = AXIS2_PLACEMENT_3D ( 'NONE', #572, #11055, #12113 ) ;
#6405 = AXIS2_PLACEMENT_3D ( 'NONE', #9652, #339, #8385 ) ;
#6406 = AXIS2_PLACEMENT_3D ( 'NONE', #9701, #12154, #311 ) ;
#6407 = EDGE_LOOP ( 'NONE', ( #3224, #8332, #2273, #14174 ) ) ;
#6408 = VERTEX_POINT ( 'NONE', #8377 ) ;
#6409 = LINE ( 'NONE', #5363, #5477 ) ;
#6410 = FACE_OUTER_BOUND ( 'NONE', #14923, .T. ) ;
#6411 = DIRECTION ( 'NONE',  ( 0.000000000000000000, 0.000000000000000000, 1.000000000000000000 ) ) ;
#6412 = ORIENTED_EDGE ( 'NONE', *, *, #10049, .F. ) ;
#6413 = ORIENTED_EDGE ( 'NONE', *, *, #2159, .F. ) ;
#6414 = CIRCLE ( 'NONE', #14200, 100.0000000000000000 ) ;
#6415 = VERTEX_POINT ( 'NONE', #8666 ) ;
#6416 = CARTESIAN_POINT ( 'NONE',  ( -68.58935777509570642, -68.58935777509452691, 8.000000000000000000 ) ) ;
#6417 = EDGE_CURVE ( 'NONE', #2568, #11548, #1933, .T. ) ;
#6418 = CARTESIAN_POINT ( 'NONE',  ( -65.58935777509570642, -68.58935777509452691, -13.00000000000000178 ) ) ;
#6419 =( LENGTH_UNIT ( ) NAMED_UNIT ( * ) SI_UNIT ( .MILLI., .METRE. ) );
#6420 = EDGE_CURVE ( 'NONE', #12891, #9888, #8003, .T. ) ;
#6421 = CARTESIAN_POINT ( 'NONE',  ( 0.000000000000000000, 0.000000000000000000, 10.50000000000000000 ) ) ;
#6422 = CIRCLE ( 'NONE', #14938, 3.000000000000002665 ) ;
#6423 = ADVANCED_FACE ( 'NONE', ( #14450 ), #13574, .T. ) ;
#6424 = ORIENTED_EDGE ( 'NONE', *, *, #12806, .T. ) ;
#6425 = COLOUR_RGB ( '', 0.66274510, 0.83137255, 0.94901961) ;
#6426 = DIRECTION ( 'NONE',  ( 0.000000000000000000, 0.000000000000000000, -1.000000000000000000 ) ) ;
#6427 = DIRECTION ( 'NONE',  ( 0.000000000000000000, 0.000000000000000000, 1.000000000000000000 ) ) ;
#6428 = ORIENTED_EDGE ( 'NONE', *, *, #6384, .F. ) ;
#6429 = ADVANCED_FACE ( 'NONE', ( #10871 ), #1402, .T. ) ;
#6430 = DIRECTION ( 'NONE',  ( 0.9557692240748186796, 0.2941176470588241498, 0.000000000000000000 ) ) ;
#6431 = VERTEX_POINT ( 'NONE', #14150 ) ;
#6432 = VERTEX_POINT ( 'NONE', #13015 ) ;
#6433 = LINE ( 'NONE', #14498, #627 ) ;
#6434 = CIRCLE ( 'NONE', #9357, 0.5000000000000004441 ) ;
#6435 = ADVANCED_FACE ( 'NONE', ( #11874 ), #13683, .F. ) ;
#6436 = DIRECTION ( 'NONE',  ( -0.000000000000000000, -0.000000000000000000, 1.000000000000000000 ) ) ;
#6437 = CARTESIAN_POINT ( 'NONE',  ( 0.000000000000000000, 0.000000000000000000, -8.000000000000000000 ) ) ;
#6438 = LINE ( 'NONE', #12231, #8967 ) ;
#6439 = ADVANCED_FACE ( 'NONE', ( #7519 ), #14685, .F. ) ;
#6440 = DIRECTION ( 'NONE',  ( 0.000000000000000000, 0.8660254037844380415, -0.5000000000000012212 ) ) ;
#6441 = EDGE_LOOP ( 'NONE', ( #13074, #11099 ) ) ;
#6442 = VECTOR ( 'NONE', #1314, 1000.000000000000000 ) ;
#6443 = CARTESIAN_POINT ( 'NONE',  ( -37.12029293941441210, -89.61631465359452875, 8.000000000000000000 ) ) ;
#6444 = PRODUCT_DEFINITION_SHAPE ( 'NONE', 'NONE',  #15031 ) ;
#6445 =( BOUNDED_SURFACE ( )  B_SPLINE_SURFACE ( 3, 2, ( 
 ( #1658, #5010, #1510 ),
 ( #1432, #13126, #3797 ),
 ( #7421, #2867, #2641 ),
 ( #7257, #12137, #11999 ),
 ( #12067, #10913, #1587 ),
 ( #517, #5150, #10993 ) ),
 .UNSPECIFIED., .F., .F., .T. ) 
 B_SPLINE_SURFACE_WITH_KNOTS ( ( 4, 2, 4 ),
 ( 3, 3 ),
 ( 0.02032853247518126918, 0.02278863295364821906, 0.02524873343211517240 ),
 ( 0.000000000000000000, 1.000000000000000000 ),
 .UNSPECIFIED. ) 
 GEOMETRIC_REPRESENTATION_ITEM ( )  RATIONAL_B_SPLINE_SURFACE ( (
 ( 1.000000000000000000, 0.8047781615896836271, 1.000000000000000000),
 ( 1.000000000000000000, 0.8123767586289616371, 1.000000000000000000),
 ( 1.000000000000000000, 0.8190662415563912946, 1.000000000000000000),
 ( 1.000000000000000000, 0.8192361015669501478, 1.000000000000000000),
 ( 1.000000000000000000, 0.8126135807103542774, 1.000000000000000000),
 ( 1.000000000000000000, 0.8047712338318590009, 1.000000000000000000) ) ) 
 REPRESENTATION_ITEM ( '' )  SURFACE ( )  );
#6446 = DIRECTION ( 'NONE',  ( 0.000000000000000000, 0.000000000000000000, 1.000000000000000000 ) ) ;
#6447 = DIRECTION ( 'NONE',  ( 1.000000000000000000, 0.000000000000000000, -0.000000000000000000 ) ) ;
#6448 = ORIENTED_EDGE ( 'NONE', *, *, #5913, .T. ) ;
#6449 = SURFACE_STYLE_USAGE ( .BOTH. , #1836 ) ;
#6450 = AXIS2_PLACEMENT_3D ( 'NONE', #751, #8783, #7796 ) ;
#6451 = VERTEX_POINT ( 'NONE', #4351 ) ;
#6452 = CARTESIAN_POINT ( 'NONE',  ( 0.000000000000000000, 0.000000000000000000, -23.50000000000000000 ) ) ;
#6453 = ORIENTED_EDGE ( 'NONE', *, *, #2576, .F. ) ;
#6454 = CIRCLE ( 'NONE', #14969, 0.5000000000000004441 ) ;
#6455 = CARTESIAN_POINT ( 'NONE',  ( -69.08004447556112382, -68.68541276968802833, -13.00000000000000178 ) ) ;
#6456 = ORIENTED_EDGE ( 'NONE', *, *, #2694, .T. ) ;
#6457 = DIRECTION ( 'NONE',  ( 1.000000000000000000, 0.000000000000000000, -0.000000000000000000 ) ) ;
#6458 = DIRECTION ( 'NONE',  ( 0.000000000000000000, 0.000000000000000000, 1.000000000000000000 ) ) ;
#6459 = CARTESIAN_POINT ( 'NONE',  ( -46.33974596215558961, 0.000000000000000000, -28.00000000000000000 ) ) ;
#6460 = DIRECTION ( 'NONE',  ( 0.000000000000000000, 0.000000000000000000, 1.000000000000000000 ) ) ;
#6461 = CARTESIAN_POINT ( 'NONE',  ( 6.917888187663118416, 52.54657765281190507, 8.000000000000000000 ) ) ;
#6462 = EDGE_CURVE ( 'NONE', #9943, #5837, #9681, .T. ) ;
#6463 = VERTEX_POINT ( 'NONE', #9878 ) ;
#6464 = EDGE_CURVE ( 'NONE', #10294, #8906, #6778, .T. ) ;
#6465 = CARTESIAN_POINT ( 'NONE',  ( -89.61631465359441506, 37.12029293941468211, -13.00000000000000178 ) ) ;
#6466 = CARTESIAN_POINT ( 'NONE',  ( 65.64523757230274725, 68.01302780753375998, -8.000000000000000000 ) ) ;
#6467 = EDGE_CURVE ( 'NONE', #11040, #9943, #9206, .T. ) ;
#6468 = ADVANCED_FACE ( 'NONE', ( #4207 ), #11258, .F. ) ;
#6469 = CARTESIAN_POINT ( 'NONE',  ( 3.999999999999998224, -2.511475576507279595, -3.469253905236645341 ) ) ;
#6470 = ORIENTED_EDGE ( 'NONE', *, *, #4326, .F. ) ;
#6471 = ADVANCED_FACE ( 'NONE', ( #7827 ), #14522, .F. ) ;
#6472 = CYLINDRICAL_SURFACE ( 'NONE', #8277, 0.5000000000000004441 ) ;
#6473 = ORIENTED_EDGE ( 'NONE', *, *, #4360, .T. ) ;
#6474 = CARTESIAN_POINT ( 'NONE',  ( 33.48561063518626923, -47.21331623427104063, -13.00000000000000178 ) ) ;
#6475 = DIRECTION ( 'NONE',  ( 0.000000000000000000, 0.000000000000000000, -1.000000000000000000 ) ) ;
#6476 = DIRECTION ( 'NONE',  ( 0.000000000000000000, 0.000000000000000000, 1.000000000000000000 ) ) ;
#6477 = DIRECTION ( 'NONE',  ( -0.000000000000000000, -0.000000000000000000, 1.000000000000000000 ) ) ;
#6478 = APPLICATION_PROTOCOL_DEFINITION ( 'draft international standard', 'automotive_design', 1998, #2615 ) ;
#6479 = ORIENTED_EDGE ( 'NONE', *, *, #14004, .T. ) ;
#6480 = ORIENTED_EDGE ( 'NONE', *, *, #12023, .T. ) ;
#6481 = EDGE_CURVE ( 'NONE', #11386, #3826, #866, .T. ) ;
#6482 = DIRECTION ( 'NONE',  ( 0.000000000000000000, 0.000000000000000000, -1.000000000000000000 ) ) ;
#6483 = CARTESIAN_POINT ( 'NONE',  ( 10.21436410913239889, 94.45034564433045432, 19.23824501837256307 ) ) ;
#6484 = CARTESIAN_POINT ( 'NONE',  ( 89.61631465359468507, -37.12029293941410657, 8.000000000000000000 ) ) ;
#6485 = ORIENTED_EDGE ( 'NONE', *, *, #7532, .F. ) ;
#6486 = AXIS2_PLACEMENT_3D ( 'NONE', #10602, #3482, #13966 ) ;
#6487 = ORIENTED_EDGE ( 'NONE', *, *, #9477, .T. ) ;
#6488 = VERTEX_POINT ( 'NONE', #11107 ) ;
#6489 = DIRECTION ( 'NONE',  ( -1.000000000000000000, 0.000000000000000000, 0.000000000000000000 ) ) ;
#6490 = CARTESIAN_POINT ( 'NONE',  ( 0.000000000000000000, 0.000000000000000000, -8.000000000000000000 ) ) ;
#6491 = FACE_OUTER_BOUND ( 'NONE', #3929, .T. ) ;
#6492 = VERTEX_POINT ( 'NONE', #939 ) ;
#6493 = DIRECTION ( 'NONE',  ( 0.000000000000000000, 0.000000000000000000, 1.000000000000000000 ) ) ;
#6494 = CARTESIAN_POINT ( 'NONE',  ( -32.65070903206048314, 101.8685403450051723, 14.31792419690431473 ) ) ;
#6495 = VERTEX_POINT ( 'NONE', #5488 ) ;
#6496 = DIRECTION ( 'NONE',  ( -0.2941176470588241498, 0.9557692240748186796, 0.000000000000000000 ) ) ;
#6497 = VERTEX_POINT ( 'NONE', #6377 ) ;
#6498 = EDGE_LOOP ( 'NONE', ( #6766, #14233, #4005, #13216, #13407, #2387, #9622, #5678 ) ) ;
#6499 = ORIENTED_EDGE ( 'NONE', *, *, #5409, .F. ) ;
#6500 = DIRECTION ( 'NONE',  ( -1.000000000000000000, 0.000000000000000000, 0.000000000000000000 ) ) ;
#6501 = EDGE_CURVE ( 'NONE', #11614, #1392, #9930, .T. ) ;
#6502 = EDGE_CURVE ( 'NONE', #8412, #13856, #11889, .T. ) ;
#6503 = ORIENTED_EDGE ( 'NONE', *, *, #8373, .F. ) ;
#6504 = DIRECTION ( 'NONE',  ( 0.000000000000000000, 0.000000000000000000, 1.000000000000000000 ) ) ;
#6505 = AXIS2_PLACEMENT_3D ( 'NONE', #1163, #13994, #12841 ) ;
#6506 = FACE_OUTER_BOUND ( 'NONE', #9509, .T. ) ;
#6507 = CARTESIAN_POINT ( 'NONE',  ( -39.30189486418265687, -33.47282819776598473, -13.00000000000000178 ) ) ;
#6508 = LINE ( 'NONE', #4337, #7004 ) ;
#6509 = VERTEX_POINT ( 'NONE', #706 ) ;
#6510 = CYLINDRICAL_SURFACE ( 'NONE', #9259, 60.50000000000000000 ) ;
#6511 = EDGE_CURVE ( 'NONE', #10004, #14269, #10682, .T. ) ;
#6512 = DIRECTION ( 'NONE',  ( 0.000000000000000000, -0.000000000000000000, -1.000000000000000000 ) ) ;
#6513 = AXIS2_PLACEMENT_3D ( 'NONE', #8419, #12003, #10844 ) ;
#6514 = DIRECTION ( 'NONE',  ( 0.000000000000000000, 0.000000000000000000, -1.000000000000000000 ) ) ;
#6515 = VERTEX_POINT ( 'NONE', #13527 ) ;
#6516 = CARTESIAN_POINT ( 'NONE',  ( 29.73684948645749415, 96.52317830260923870, -11.65681975620353406 ) ) ;
#6517 = EDGE_CURVE ( 'NONE', #8372, #11582, #9692, .T. ) ;
#6518 = ADVANCED_FACE ( 'NONE', ( #2982 ), #7604, .F. ) ;
#6519 = ORIENTED_EDGE ( 'NONE', *, *, #5695, .T. ) ;
#6520 = LINE ( 'NONE', #6598, #2769 ) ;
#6521 = ORIENTED_EDGE ( 'NONE', *, *, #13254, .T. ) ;
#6522 = LINE ( 'NONE', #2136, #2185 ) ;
#6523 = VERTEX_POINT ( 'NONE', #7683 ) ;
#6524 = DIRECTION ( 'NONE',  ( 0.000000000000000000, 0.000000000000000000, -1.000000000000000000 ) ) ;
#6526 = DIRECTION ( 'NONE',  ( 0.000000000000000000, 0.000000000000000000, -1.000000000000000000 ) ) ;
#6525 = AXIS2_PLACEMENT_3D ( 'NONE', #6995, #10430, #4750 ) ;
#6527 = CARTESIAN_POINT ( 'NONE',  ( 0.000000000000000000, 0.000000000000000000, 10.50000000000000000 ) ) ;
#6528 = EDGE_CURVE ( 'NONE', #8812, #8852, #7559, .T. ) ;
#6529 = AXIS2_PLACEMENT_3D ( 'NONE', #2836, #13303, #473 ) ;
#6530 = DIRECTION ( 'NONE',  ( 0.000000000000000000, 0.000000000000000000, 1.000000000000000000 ) ) ;
#6532 = CARTESIAN_POINT ( 'NONE',  ( -6.917888187662729393, -52.54657765281195481, -10.50000000000000000 ) ) ;
#6531 = CIRCLE ( 'NONE', #7991, 3.000000000000002665 ) ;
#6533 =( BOUNDED_SURFACE ( )  B_SPLINE_SURFACE ( 3, 2, ( 
 ( #9821, #14535, #5274 ),
 ( #8679, #12270, #4143 ),
 ( #13398, #1859, #10740 ),
 ( #8907, #3303, #4300 ),
 ( #7842, #11200, #6622 ),
 ( #13704, #2083, #14621 ) ),
 .UNSPECIFIED., .F., .F., .T. ) 
 B_SPLINE_SURFACE_WITH_KNOTS ( ( 4, 2, 4 ),
 ( 3, 3 ),
 ( 0.02032853247518126918, 0.02278863295364821906, 0.02524873343211516893 ),
 ( 0.000000000000000000, 1.000000000000000000 ),
 .UNSPECIFIED. ) 
 GEOMETRIC_REPRESENTATION_ITEM ( )  RATIONAL_B_SPLINE_SURFACE ( (
 ( 1.000000000000000000, 0.8047781615896838492, 1.000000000000000000),
 ( 1.000000000000000000, 0.8123767586290684406, 1.000000000000000000),
 ( 1.000000000000000000, 0.8190662415562490750, 1.000000000000000000),
 ( 1.000000000000000000, 0.8192361015670930335, 1.000000000000000000),
 ( 1.000000000000000000, 0.8126135807102463637, 1.000000000000000000),
 ( 1.000000000000000000, 0.8047712338318585568, 1.000000000000000000) ) ) 
 REPRESENTATION_ITEM ( '' )  SURFACE ( )  );
#6534 = DIRECTION ( 'NONE',  ( 1.000000000000000000, 0.000000000000000000, 0.000000000000000000 ) ) ;
#6535 = ORIENTED_EDGE ( 'NONE', *, *, #7034, .F. ) ;
#6536 = CARTESIAN_POINT ( 'NONE',  ( 11.10403672352021331, 74.17481381252333961, -18.51301757891052091 ) ) ;
#6537 = CARTESIAN_POINT ( 'NONE',  ( 25.00000000000000000, 81.24038404635960831, 31.00000000000000000 ) ) ;
#6538 = AXIS2_PLACEMENT_3D ( 'NONE', #7679, #3207, #10262 ) ;
#6539 = CARTESIAN_POINT ( 'NONE',  ( 3.999999999999999112, 0.8228435280417655262, -3.430609588141304123 ) ) ;
#6540 = ORIENTED_EDGE ( 'NONE', *, *, #9620, .T. ) ;
#6541 = DIRECTION ( 'NONE',  ( 0.000000000000000000, 0.000000000000000000, -1.000000000000000000 ) ) ;
#6542 = EDGE_LOOP ( 'NONE', ( #9046, #5304, #13728, #9199, #2893 ) ) ;
#6543 = EDGE_CURVE ( 'NONE', #6775, #2732, #10921, .T. ) ;
#6544 = DIRECTION ( 'NONE',  ( -0.000000000000000000, -0.000000000000000000, 1.000000000000000000 ) ) ;
#6545 = DIRECTION ( 'NONE',  ( 1.000000000000000000, 0.000000000000000000, 0.000000000000000000 ) ) ;
#6546 = AXIS2_PLACEMENT_3D ( 'NONE', #5008, #3861, #14331 ) ;
#6547 = EDGE_CURVE ( 'NONE', #11546, #1207, #13586, .T. ) ;
#6548 = DIRECTION ( 'NONE',  ( 0.000000000000000000, 0.000000000000000000, 1.000000000000000000 ) ) ;
#6549 = CARTESIAN_POINT ( 'NONE',  ( -52.04657765281192638, 6.917888187662934563, -10.50000000000000000 ) ) ;
#6550 = DIRECTION ( 'NONE',  ( 6.123233995736766036E-17, 0.000000000000000000, 1.000000000000000000 ) ) ;
#6551 = VERTEX_POINT ( 'NONE', #5627 ) ;
#6552 = ADVANCED_BREP_SHAPE_REPRESENTATION ( '', ( #9343, #5108 ), #10652 ) ;
#6553 = VECTOR ( 'NONE', #5742, 1000.000000000000000 ) ;
#6554 = EDGE_LOOP ( 'NONE', ( #11534, #9356, #7322, #9108, #10154, #7526, #7007, #9419, #3079, #12109 ) ) ;
#6555 = ORIENTED_EDGE ( 'NONE', *, *, #5772, .T. ) ;
#6556 = AXIS2_PLACEMENT_3D ( 'NONE', #7716, #6573, #8865 ) ;
#6557 = ADVANCED_FACE ( 'NONE', ( #8 ), #85, .F. ) ;
#6558 = CARTESIAN_POINT ( 'NONE',  ( -19.99999999999998224, 64.99230723708768664, 26.00000000000000000 ) ) ;
#6559 = CARTESIAN_POINT ( 'NONE',  ( 34.93865171984692353, 100.8681255216228436, 15.83776386865434382 ) ) ;
#6560 = DIRECTION ( 'NONE',  ( 0.000000000000000000, 0.000000000000000000, 1.000000000000000000 ) ) ;
#6561 = VERTEX_POINT ( 'NONE', #9341 ) ;
#6562 = AXIS2_PLACEMENT_3D ( 'NONE', #14647, #12296, #7568 ) ;
#6563 = ORIENTED_EDGE ( 'NONE', *, *, #13638, .T. ) ;
#6564 = AXIS2_PLACEMENT_3D ( 'NONE', #10506, #5867, #11517 ) ;
#6565 = EDGE_CURVE ( 'NONE', #11838, #3039, #4152, .T. ) ;
#6566 = ORIENTED_EDGE ( 'NONE', *, *, #9964, .F. ) ;
#6567 = EDGE_CURVE ( 'NONE', #6561, #7296, #4391, .T. ) ;
#6568 = CIRCLE ( 'NONE', #4418, 0.5000000000000004441 ) ;
#6569 = DIRECTION ( 'NONE',  ( 0.000000000000000000, 0.000000000000000000, 1.000000000000000000 ) ) ;
#6570 = CYLINDRICAL_SURFACE ( 'NONE', #4697, 2.649999999999992806 ) ;
#6571 = CYLINDRICAL_SURFACE ( 'NONE', #552, 14.00000000000000000 ) ;
#6572 = ORIENTED_EDGE ( 'NONE', *, *, #4069, .T. ) ;
#6574 = COLOUR_RGB ( '', 0.31764706, 0.68627451, 0.89019608) ;
#6573 = DIRECTION ( 'NONE',  ( 0.000000000000000000, 0.000000000000000000, 1.000000000000000000 ) ) ;
#6575 = DIRECTION ( 'NONE',  ( 0.000000000000000000, 1.000000000000000000, -0.000000000000000000 ) ) ;
#6576 = VERTEX_POINT ( 'NONE', #8058 ) ;
#6577 = B_SPLINE_CURVE_WITH_KNOTS ( 'NONE', 3,
 ( #10136, #7472, #1798, #9988, #12348, #11063 ),
 .UNSPECIFIED., .F., .F.,
 ( 4, 2, 4 ),
 ( -3.640115492404583136E-06, 0.0002066546034003430006, 0.0004169493222930905534 ),
 .UNSPECIFIED. ) ;
#6578 = DIRECTION ( 'NONE',  ( 0.000000000000000000, 0.000000000000000000, 1.000000000000000000 ) ) ;
#6579 = AXIS2_PLACEMENT_3D ( 'NONE', #11769, #3717, #13320 ) ;
#6580 = ORIENTED_EDGE ( 'NONE', *, *, #11918, .T. ) ;
#6581 = ORIENTED_EDGE ( 'NONE', *, *, #14792, .T. ) ;
#6582 = CARTESIAN_POINT ( 'NONE',  ( -45.89934640057513349, 26.50000000000019540, -13.00000000000000178 ) ) ;
#6583 = DIRECTION ( 'NONE',  ( 1.000000000000000000, 0.000000000000000000, 0.000000000000000000 ) ) ;
#6584 = CIRCLE ( 'NONE', #9739, 50.00000000000000000 ) ;
#6585 = CARTESIAN_POINT ( 'NONE',  ( 94.51066581171355097, 1.674280531758986834, -8.000000000000000000 ) ) ;
#6586 = CARTESIAN_POINT ( 'NONE',  ( 0.000000000000000000, 0.000000000000000000, -10.50000000000000000 ) ) ;
#6587 = DIRECTION ( 'NONE',  ( -1.000000000000000000, 0.000000000000000000, 0.000000000000000000 ) ) ;
#6588 = ORIENTED_EDGE ( 'NONE', *, *, #11370, .F. ) ;
#6589 = DIRECTION ( 'NONE',  ( 0.000000000000000000, 0.000000000000000000, 1.000000000000000000 ) ) ;
#6590 = CIRCLE ( 'NONE', #12436, 3.000000000000004441 ) ;
#6591 = CARTESIAN_POINT ( 'NONE',  ( -14.07862063237857342, 50.84834283437004387, -13.00000000000000178 ) ) ;
#6592 = CARTESIAN_POINT ( 'NONE',  ( -3.492805317593278058, 46.55633131742322917, -10.50000000000000000 ) ) ;
#6593 = AXIS2_PLACEMENT_3D ( 'NONE', #2222, #12697, #1092 ) ;
#6594 = VERTEX_POINT ( 'NONE', #3438 ) ;
#6595 = CARTESIAN_POINT ( 'NONE',  ( 33.38013186279886924, 95.32466787866007962, -15.87266497586409209 ) ) ;
#6596 = ORIENTED_EDGE ( 'NONE', *, *, #2830, .F. ) ;
#6597 = VECTOR ( 'NONE', #14167, 1000.000000000000000 ) ;
#6598 = CARTESIAN_POINT ( 'NONE',  ( -7.499999999999996447, 85.00000000000000000, 46.00000000000000000 ) ) ;
#6599 = EDGE_LOOP ( 'NONE', ( #13669, #14595, #2236 ) ) ;
#6600 = DIRECTION ( 'NONE',  ( 0.000000000000000000, 0.000000000000000000, 1.000000000000000000 ) ) ;
#6601 = CIRCLE ( 'NONE', #9281, 4.999999999999995559 ) ;
#6602 = ORIENTED_EDGE ( 'NONE', *, *, #12574, .T. ) ;
#6603 = DIRECTION ( 'NONE',  ( 0.000000000000000000, 0.000000000000000000, 1.000000000000000000 ) ) ;
#6604 = CARTESIAN_POINT ( 'NONE',  ( 87.95718916809192933, -34.62083247296232713, -13.00000000000000178 ) ) ;
#6605 = FACE_OUTER_BOUND ( 'NONE', #12330, .T. ) ;
#6606 = VECTOR ( 'NONE', #2747, 1000.000000000000000 ) ;
#6607 = EDGE_LOOP ( 'NONE', ( #12243, #13803, #912 ) ) ;
#6608 = CARTESIAN_POINT ( 'NONE',  ( -12.50000000000000000, 106.2673515243510991, -15.00000000000000000 ) ) ;
#6609 = EDGE_CURVE ( 'NONE', #2014, #9738, #4626, .T. ) ;
#6610 = DIRECTION ( 'NONE',  ( 1.000000000000000000, 0.000000000000000000, 0.000000000000000000 ) ) ;
#6611 = EDGE_CURVE ( 'NONE', #5951, #964, #14979, .T. ) ;
#6612 = EDGE_CURVE ( 'NONE', #836, #3842, #12630, .T. ) ;
#6613 = CARTESIAN_POINT ( 'NONE',  ( 0.000000000000000000, 4.862606272033088928, -3.745885042887437510 ) ) ;
#6614 = VECTOR ( 'NONE', #8839, 1000.000000000000000 ) ;
#6615 = ORIENTED_EDGE ( 'NONE', *, *, #14715, .T. ) ;
#6616 = CARTESIAN_POINT ( 'NONE',  ( 68.49330278050122445, -68.09867107463004743, -13.00000000000000178 ) ) ;
#6617 = CARTESIAN_POINT ( 'NONE',  ( -52.54657765281192638, 6.917888187662934563, -13.00000000000000178 ) ) ;
#6618 = AXIS2_PLACEMENT_3D ( 'NONE', #14596, #3054, #4196 ) ;
#6619 = FACE_OUTER_BOUND ( 'NONE', #782, .T. ) ;
#6620 = CARTESIAN_POINT ( 'NONE',  ( -25.00000000000000000, 81.24038404635962252, -26.00000000000000000 ) ) ;
#6621 = EDGE_LOOP ( 'NONE', ( #3088, #5302, #14385, #9902 ) ) ;
#6622 = CARTESIAN_POINT ( 'NONE',  ( -0.6810597143197720804, -4.461075778259609770, -3.598441714920719292 ) ) ;
#6623 = CIRCLE ( 'NONE', #12454, 18.00000000000000355 ) ;
#6624 = ORIENTED_EDGE ( 'NONE', *, *, #8286, .T. ) ;
#6625 = CARTESIAN_POINT ( 'NONE',  ( 9.706953719245472456, 57.06275842387054098, -13.00000000000000178 ) ) ;
#6626 = DIRECTION ( 'NONE',  ( 0.000000000000000000, 0.000000000000000000, -1.000000000000000000 ) ) ;
#6627 = DIRECTION ( 'NONE',  ( -0.000000000000000000, -0.000000000000000000, 1.000000000000000000 ) ) ;
#6628 = DIRECTION ( 'NONE',  ( 1.000000000000000000, 0.000000000000000000, 0.000000000000000000 ) ) ;
#6629 = CONTEXT_DEPENDENT_SHAPE_REPRESENTATION ( #6198, #3915 ) ;
#6630 = ORIENTED_EDGE ( 'NONE', *, *, #10346, .T. ) ;
#6631 = VERTEX_POINT ( 'NONE', #2221 ) ;
#6632 = EDGE_LOOP ( 'NONE', ( #3744, #2449, #160, #2583 ) ) ;
#6633 = AXIS2_PLACEMENT_3D ( 'NONE', #9951, #13376, #4049 ) ;
#6634 = VECTOR ( 'NONE', #6340, 1000.000000000000000 ) ;
#6635 = CARTESIAN_POINT ( 'NONE',  ( 68.58935777509523746, 68.58935777509499587, -10.50000000000000000 ) ) ;
#6636 = CARTESIAN_POINT ( 'NONE',  ( 31.95875033779849872, 102.1112180006092984, 13.22918226575834311 ) ) ;
#6637 = CIRCLE ( 'NONE', #1082, 60.50000000000000000 ) ;
#6638 = EDGE_CURVE ( 'NONE', #8983, #8663, #10265, .T. ) ;
#6639 = CARTESIAN_POINT ( 'NONE',  ( 41.94820822869167642, 33.29654390035863543, -10.50000000000000000 ) ) ;
#6640 = ORIENTED_EDGE ( 'NONE', *, *, #8025, .F. ) ;
#6641 = ORIENTED_EDGE ( 'NONE', *, *, #2437, .F. ) ;
#6642 = CIRCLE ( 'NONE', #2302, 60.50000000000000000 ) ;
#6643 = EDGE_LOOP ( 'NONE', ( #12363, #11650, #7639, #11707, #2245 ) ) ;
#6644 = AXIS2_PLACEMENT_3D ( 'NONE', #14873, #9312, #7946 ) ;
#6645 = CARTESIAN_POINT ( 'NONE',  ( -12.50000000000000000, 100.2235002382176248, -15.00000000000000000 ) ) ;
#6646 = CIRCLE ( 'NONE', #10776, 2.649999999999992806 ) ;
#6647 = DIRECTION ( 'NONE',  ( 0.000000000000000000, 0.000000000000000000, 1.000000000000000000 ) ) ;
#6648 = DIRECTION ( 'NONE',  ( 0.000000000000000000, 0.000000000000000000, 1.000000000000000000 ) ) ;
#6649 = DIRECTION ( 'NONE',  ( -0.000000000000000000, -0.000000000000000000, 1.000000000000000000 ) ) ;
#6650 = ORIENTED_EDGE ( 'NONE', *, *, #83, .T. ) ;
#6651 = CARTESIAN_POINT ( 'NONE',  ( 53.55662432702593634, -6.558794855522958910E-15, -10.50000000000000000 ) ) ;
#6652 = CARTESIAN_POINT ( 'NONE',  ( 19.68583958711425552, -30.74264578624780597, -25.50000000000000355 ) ) ;
#6653 = VERTEX_POINT ( 'NONE', #8134 ) ;
#6655 = EDGE_CURVE ( 'NONE', #7623, #2264, #8103, .T. ) ;
#6654 = DIRECTION ( 'NONE',  ( 0.000000000000000000, 0.000000000000000000, 1.000000000000000000 ) ) ;
#6656 = VECTOR ( 'NONE', #6745, 999.9999999999998863 ) ;
#6657 = EDGE_CURVE ( 'NONE', #4183, #13408, #12864, .T. ) ;
#6658 = AXIS2_PLACEMENT_3D ( 'NONE', #349, #9596, #9660 ) ;
#6659 = VERTEX_POINT ( 'NONE', #10485 ) ;
#6660 = AXIS2_PLACEMENT_3D ( 'NONE', #9188, #5922, #8357 ) ;
#6661 = ORIENTED_EDGE ( 'NONE', *, *, #5367, .T. ) ;
#6662 = DIRECTION ( 'NONE',  ( 0.000000000000000000, 0.000000000000000000, -1.000000000000000000 ) ) ;
#6663 = CARTESIAN_POINT ( 'NONE',  ( -13.71740939043329277, 51.19406879332069593, 8.000000000000000000 ) ) ;
#6664 = EDGE_CURVE ( 'NONE', #8869, #11469, #2200, .T. ) ;
#6665 = CARTESIAN_POINT ( 'NONE',  ( 5.200000000000006395, 3.061616997868349122E-16, -2.499999999999972911 ) ) ;
#6666 = AXIS2_PLACEMENT_3D ( 'NONE', #384, #6134, #5021 ) ;
#6667 = DIRECTION ( 'NONE',  ( 1.000000000000000000, 0.000000000000000000, 0.000000000000000000 ) ) ;
#6668 = LINE ( 'NONE', #12456, #5582 ) ;
#6669 = CIRCLE ( 'NONE', #3539, 4.250000000000000000 ) ;
#6670 = CARTESIAN_POINT ( 'NONE',  ( 0.000000000000000000, 0.000000000000000000, -10.50000000000000000 ) ) ;
#6671 = ORIENTED_EDGE ( 'NONE', *, *, #12649, .F. ) ;
#6672 = CARTESIAN_POINT ( 'NONE',  ( 2.500000000000002220, 2.357898499370430834, -6.938893903907228378E-15 ) ) ;
#6673 = EDGE_CURVE ( 'NONE', #13021, #2940, #6068, .T. ) ;
#6674 = AXIS2_PLACEMENT_3D ( 'NONE', #2331, #13802, #13884 ) ;
#6675 = DIRECTION ( 'NONE',  ( -0.000000000000000000, -0.000000000000000000, 1.000000000000000000 ) ) ;
#6676 = CARTESIAN_POINT ( 'NONE',  ( 1.393927851585481159, -4.043713361053541178, -3.526374918436839145 ) ) ;
#6677 = AXIS2_PLACEMENT_3D ( 'NONE', #13139, #14049, #12992 ) ;
#6678 = ORIENTED_EDGE ( 'NONE', *, *, #9759, .T. ) ;
#6679 = DIRECTION ( 'NONE',  ( 0.000000000000000000, 0.000000000000000000, -1.000000000000000000 ) ) ;
#6680 = VERTEX_POINT ( 'NONE', #13068 ) ;
#6681 = FACE_OUTER_BOUND ( 'NONE', #9838, .T. ) ;
#6682 = ORIENTED_EDGE ( 'NONE', *, *, #2631, .F. ) ;
#6683 = DIRECTION ( 'NONE',  ( 0.000000000000000000, 0.000000000000000000, 1.000000000000000000 ) ) ;
#6684 = DIRECTION ( 'NONE',  ( -1.000000000000000000, 0.000000000000000000, 0.000000000000000000 ) ) ;
#6685 = DIRECTION ( 'NONE',  ( -1.000000000000000000, 0.000000000000000000, 0.000000000000000000 ) ) ;
#6686 = CARTESIAN_POINT ( 'NONE',  ( 68.58935777509475429, -68.58935777509547904, 10.49999999999999822 ) ) ;
#6687 = CIRCLE ( 'NONE', #8149, 3.000000000000002665 ) ;
#6688 = CARTESIAN_POINT ( 'NONE',  ( -12.86891638962156215, 56.43380494353993271, 10.49999999999999822 ) ) ;
#6689 = CARTESIAN_POINT ( 'NONE',  ( -10.88080562889580705, 74.20685544768620900, -18.69467976711750978 ) ) ;
#6690 = CARTESIAN_POINT ( 'NONE',  ( 0.000000000000000000, -4.618802153517023612, -5.000000000000000888 ) ) ;
#6691 = ORIENTED_EDGE ( 'NONE', *, *, #11166, .F. ) ;
#6692 = DIRECTION ( 'NONE',  ( -1.000000000000000000, 0.000000000000000000, 0.000000000000000000 ) ) ;
#6693 = DIRECTION ( 'NONE',  ( 0.000000000000000000, 0.000000000000000000, -1.000000000000000000 ) ) ;
#6694 = DIRECTION ( 'NONE',  ( 0.000000000000000000, 0.000000000000000000, -1.000000000000000000 ) ) ;
#6695 = CIRCLE ( 'NONE', #14720, 56.99999999999998579 ) ;
#6696 = CYLINDRICAL_SURFACE ( 'NONE', #3524, 56.99999999999999289 ) ;
#6697 = ORIENTED_EDGE ( 'NONE', *, *, #2089, .F. ) ;
#6698 = EDGE_CURVE ( 'NONE', #836, #4561, #1228, .T. ) ;
#6699 = DIRECTION ( 'NONE',  ( 1.000000000000000000, 0.000000000000000000, 0.000000000000000000 ) ) ;
#6700 = EDGE_CURVE ( 'NONE', #7016, #3633, #499, .T. ) ;
#6701 = ORIENTED_EDGE ( 'NONE', *, *, #14248, .T. ) ;
#6702 = CARTESIAN_POINT ( 'NONE',  ( 0.000000000000000000, 0.000000000000000000, 20.00000000000000000 ) ) ;
#6703 = DIRECTION ( 'NONE',  ( 0.000000000000000000, 0.000000000000000000, 1.000000000000000000 ) ) ;
#6704 = ORIENTED_EDGE ( 'NONE', *, *, #458, .T. ) ;
#6705 = CARTESIAN_POINT ( 'NONE',  ( 9.260566377415146988, 106.5986160369160558, -19.68264575353697055 ) ) ;
#6706 = CARTESIAN_POINT ( 'NONE',  ( -0.6666666666666659635, 4.233901974057258322, -3.300726591567080703 ) ) ;
#6707 = ITEM_DEFINED_TRANSFORMATION ( 'NONE', 'NONE', #14059,  #5108 ) ;
#6708 = ORIENTED_EDGE ( 'NONE', *, *, #11227, .F. ) ;
#6709 = ORIENTED_EDGE ( 'NONE', *, *, #6609, .F. ) ;
#6710 = CARTESIAN_POINT ( 'NONE',  ( -12.28299983316191302, 61.79111512501306436, -16.56818193787248816 ) ) ;
#6711 = CARTESIAN_POINT ( 'NONE',  ( 31.47058823529414440, 102.2673069760056421, 11.33188329630078783 ) ) ;
#6712 = LINE ( 'NONE', #14779, #4466 ) ;
#6713 = VERTEX_POINT ( 'NONE', #5085 ) ;
#6714 = ORIENTED_EDGE ( 'NONE', *, *, #14511, .F. ) ;
#6715 = EDGE_CURVE ( 'NONE', #14819, #7570, #2659, .T. ) ;
#6716 = ORIENTED_EDGE ( 'NONE', *, *, #8401, .F. ) ;
#6717 = DIRECTION ( 'NONE',  ( -1.000000000000000000, 0.000000000000000000, 0.000000000000000000 ) ) ;
#6718 = FACE_OUTER_BOUND ( 'NONE', #5541, .T. ) ;
#6719 = CARTESIAN_POINT ( 'NONE',  ( 92.61631465359468507, -37.12029293941410657, -8.000000000000000000 ) ) ;
#6720 = PRESENTATION_STYLE_ASSIGNMENT (( #10376 ) ) ;
#6721 = CARTESIAN_POINT ( 'NONE',  ( 12.86891638962116247, -56.43380494354001087, -13.00000000000000178 ) ) ;
#6722 = PLANE ( 'NONE',  #2226 ) ;
#6723 = ORIENTED_EDGE ( 'NONE', *, *, #7949, .T. ) ;
#6724 = DIRECTION ( 'NONE',  ( -0.000000000000000000, -0.000000000000000000, 1.000000000000000000 ) ) ;
#6725 = AXIS2_PLACEMENT_3D ( 'NONE', #11758, #1423, #11686 ) ;
#6726 = VERTEX_POINT ( 'NONE', #7279 ) ;
#6727 = ORIENTED_EDGE ( 'NONE', *, *, #7008, .F. ) ;
#6728 = PLANE ( 'NONE',  #4513 ) ;
#6729 = ORIENTED_EDGE ( 'NONE', *, *, #8145, .T. ) ;
#6730 = CARTESIAN_POINT ( 'NONE',  ( 29.70588235294119173, 96.53269163155674448, -79.80561291909842225 ) ) ;
#6731 = ADVANCED_FACE ( 'NONE', ( #9702 ), #10856, .F. ) ;
#6732 = DIRECTION ( 'NONE',  ( -0.000000000000000000, -0.000000000000000000, 1.000000000000000000 ) ) ;
#6733 = ADVANCED_FACE ( 'NONE', ( #9630 ), #14131, .F. ) ;
#6734 = EDGE_CURVE ( 'NONE', #1622, #11466, #6215, .T. ) ;
#6735 = LINE ( 'NONE', #11391, #9814 ) ;
#6736 = FACE_OUTER_BOUND ( 'NONE', #6386, .T. ) ;
#6737 = DIRECTION ( 'NONE',  ( -0.000000000000000000, -0.000000000000000000, -1.000000000000000000 ) ) ;
#6738 = VERTEX_POINT ( 'NONE', #14350 ) ;
#6739 = DIRECTION ( 'NONE',  ( 0.000000000000000000, 0.8660254037844389297, 0.4999999999999995559 ) ) ;
#6740 = ORIENTED_EDGE ( 'NONE', *, *, #6900, .T. ) ;
#6741 = EDGE_CURVE ( 'NONE', #8488, #13671, #8570, .T. ) ;
#6742 = DIRECTION ( 'NONE',  ( 0.000000000000000000, 0.000000000000000000, 1.000000000000000000 ) ) ;
#6743 = DIRECTION ( 'NONE',  ( -0.000000000000000000, -0.000000000000000000, -1.000000000000000000 ) ) ;
#6744 = ORIENTED_EDGE ( 'NONE', *, *, #14274, .T. ) ;
#6745 = DIRECTION ( 'NONE',  ( 0.8191520442889875797, 0.000000000000000000, 0.5735764363510522656 ) ) ;
#6746 = CARTESIAN_POINT ( 'NONE',  ( 3.999999999999997335, 1.941961291383485388, -0.3515519931180224322 ) ) ;
#6747 = FACE_OUTER_BOUND ( 'NONE', #2102, .T. ) ;
#6748 = EDGE_CURVE ( 'NONE', #11386, #11838, #10194, .T. ) ;
#6749 = ADVANCED_FACE ( 'NONE', ( #13145 ), #8431, .F. ) ;
#6750 = CARTESIAN_POINT ( 'NONE',  ( -2.449293598294700991E-16, 97.00000000000000000, 8.000000000000000000 ) ) ;
#6751 = CARTESIAN_POINT ( 'NONE',  ( -12.49999999999999645, 106.2673515243510849, 15.33085973118639167 ) ) ;
#6752 = FACE_OUTER_BOUND ( 'NONE', #13558, .T. ) ;
#6753 = DIRECTION ( 'NONE',  ( 0.000000000000000000, 0.000000000000000000, 1.000000000000000000 ) ) ;
#6754 = CARTESIAN_POINT ( 'NONE',  ( -12.34196858416779996, 73.97755844198597686, -16.27929523640516862 ) ) ;
#6755 = AXIS2_PLACEMENT_3D ( 'NONE', #9705, #1530, #3959 ) ;
#6756 = DIRECTION ( 'NONE',  ( -1.000000000000000000, 0.000000000000000000, 0.000000000000000000 ) ) ;
#6757 = ORIENTED_EDGE ( 'NONE', *, *, #5000, .T. ) ;
#6758 = CARTESIAN_POINT ( 'NONE',  ( 68.58935777509475429, -68.58935777509547904, 8.000000000000000000 ) ) ;
#6759 = CARTESIAN_POINT ( 'NONE',  ( 68.01302780753354682, -65.64523757230297463, -8.000000000000000000 ) ) ;
#6760 = CYLINDRICAL_SURFACE ( 'NONE', #9513, 3.000000000000002665 ) ;
#6761 = AXIS2_PLACEMENT_3D ( 'NONE', #524, #12072, #9767 ) ;
#6762 = CARTESIAN_POINT ( 'NONE',  ( 3.678949249685234957, 0.000000000000000000, 0.000000000000000000 ) ) ;
#6763 = EDGE_LOOP ( 'NONE', ( #13353, #12260, #2034, #4699 ) ) ;
#6764 = FACE_OUTER_BOUND ( 'NONE', #6964, .T. ) ;
#6765 = CIRCLE ( 'NONE', #6513, 0.5000000000000004441 ) ;
#6766 = ORIENTED_EDGE ( 'NONE', *, *, #4800, .F. ) ;
#6767 = AXIS2_PLACEMENT_3D ( 'NONE', #5166, #9934, #1895 ) ;
#6768 = PLANE ( 'NONE',  #2538 ) ;
#6769 = SURFACE_STYLE_USAGE ( .BOTH. , #7925 ) ;
#6770 = CARTESIAN_POINT ( 'NONE',  ( 8.791121401460923579, 106.6383652286472881, -19.83320147728688454 ) ) ;
#6771 = CARTESIAN_POINT ( 'NONE',  ( 12.86891638962116247, -56.43380494354001087, -13.00000000000000178 ) ) ;
#6772 = ORIENTED_EDGE ( 'NONE', *, *, #3017, .T. ) ;
#6773 = PRODUCT_DEFINITION_FORMATION_WITH_SPECIFIED_SOURCE ( 'ANY', '', #5123, .NOT_KNOWN. ) ;
#6774 = AXIS2_PLACEMENT_3D ( 'NONE', #5768, #4725, #13989 ) ;
#6775 = VERTEX_POINT ( 'NONE', #9484 ) ;
#6776 = EDGE_CURVE ( 'NONE', #2714, #7044, #9461, .T. ) ;
#6777 = CARTESIAN_POINT ( 'NONE',  ( 44.79355920668812274, 31.05588327715851449, 8.000000000000000000 ) ) ;
#6778 = CIRCLE ( 'NONE', #987, 63.00000000000000000 ) ;
#6779 = CARTESIAN_POINT ( 'NONE',  ( 8.635722793752535154, 94.60824746434937538, 19.90313979694426649 ) ) ;
#6780 =( GEOMETRIC_REPRESENTATION_CONTEXT ( 3 ) GLOBAL_UNCERTAINTY_ASSIGNED_CONTEXT ( ( #765 ) ) GLOBAL_UNIT_ASSIGNED_CONTEXT ( ( #9684, #8555, #9542 ) ) REPRESENTATION_CONTEXT ( 'NONE', 'WORKASPACE' ) );
#6781 = CARTESIAN_POINT ( 'NONE',  ( -52.36539807335606156, 6.451868917687758831, 10.49999999999999822 ) ) ;
#6782 = ORIENTED_EDGE ( 'NONE', *, *, #8673, .T. ) ;
#6783 = ORIENTED_EDGE ( 'NONE', *, *, #5907, .F. ) ;
#6784 = AXIS2_PLACEMENT_3D ( 'NONE', #4107, #1678, #7363 ) ;
#6785 = ORIENTED_EDGE ( 'NONE', *, *, #7198, .T. ) ;
#6786 = AXIS2_PLACEMENT_3D ( 'NONE', #13661, #7886, #11008 ) ;
#6787 = CARTESIAN_POINT ( 'NONE',  ( 8.914534555419061590, 74.46880876796768689, 19.80411369943039901 ) ) ;
#6788 = AXIS2_PLACEMENT_3D ( 'NONE', #5331, #9958, #14607 ) ;
#6790 = AXIS2_PLACEMENT_3D ( 'NONE', #6592, #6364, #6447 ) ;
#6789 = DIRECTION ( 'NONE',  ( -0.000000000000000000, -0.000000000000000000, -1.000000000000000000 ) ) ;
#6791 = AXIS2_PLACEMENT_3D ( 'NONE', #8758, #1709, #10886 ) ;
#6792 = DIRECTION ( 'NONE',  ( 0.000000000000000000, 1.000000000000000000, -1.224646799147353207E-16 ) ) ;
#6793 = SURFACE_STYLE_FILL_AREA ( #12740 ) ;
#6794 = CARTESIAN_POINT ( 'NONE',  ( 89.61631465359468507, -37.12029293941410657, 8.000000000000000000 ) ) ;
#6795 = ORIENTED_EDGE ( 'NONE', *, *, #4726, .F. ) ;
#6796 = FACE_OUTER_BOUND ( 'NONE', #11905, .T. ) ;
#6797 = ORIENTED_EDGE ( 'NONE', *, *, #5083, .F. ) ;
#6798 = EDGE_CURVE ( 'NONE', #11834, #259, #2929, .T. ) ;
#6799 = EDGE_CURVE ( 'NONE', #1338, #11078, #5105, .T. ) ;
#6800 = ADVANCED_FACE ( 'NONE', ( #8358 ), #4872, .T. ) ;
#6801 = CIRCLE ( 'NONE', #11434, 56.99999999999999289 ) ;
#6802 = FACE_OUTER_BOUND ( 'NONE', #3006, .T. ) ;
#6803 = CARTESIAN_POINT ( 'NONE',  ( 0.000000000000000000, 0.000000000000000000, 8.000000000000000000 ) ) ;
#6804 = CIRCLE ( 'NONE', #9950, 56.99999999999999289 ) ;
#6805 = VERTEX_POINT ( 'NONE', #8279 ) ;
#6806 = AXIS2_PLACEMENT_3D ( 'NONE', #3697, #15013, #12956 ) ;
#6807 = AXIS2_PLACEMENT_3D ( 'NONE', #3223, #13618, #1029 ) ;
#6808 = ORIENTED_EDGE ( 'NONE', *, *, #252, .T. ) ;
#6809 = CARTESIAN_POINT ( 'NONE',  ( 2.449293598294700991E-16, -97.00000000000000000, -10.50000000000000000 ) ) ;
#6810 = EDGE_CURVE ( 'NONE', #11429, #8704, #1385, .T. ) ;
#6811 = CYLINDRICAL_SURFACE ( 'NONE', #12628, 60.50000000000000000 ) ;
#6812 = DIRECTION ( 'NONE',  ( 0.000000000000000000, 0.000000000000000000, 1.000000000000000000 ) ) ;
#6813 = CIRCLE ( 'NONE', #8509, 3.000000000000002665 ) ;
#6814 = CARTESIAN_POINT ( 'NONE',  ( -0.3208286057739655472, 4.433571671609678688, -0.3503314178412536006 ) ) ;
#6815 = DIRECTION ( 'NONE',  ( -1.000000000000000000, 0.000000000000000000, 0.000000000000000000 ) ) ;
#6816 = CARTESIAN_POINT ( 'NONE',  ( 22.33583958711425055, -30.74264578624780597, -25.50000000000000355 ) ) ;
#6817 = AXIS2_PLACEMENT_3D ( 'NONE', #8835, #6475, #4448 ) ;
#6818 = ORIENTED_EDGE ( 'NONE', *, *, #13781, .T. ) ;
#6819 = CARTESIAN_POINT ( 'NONE',  ( 0.000000000000000000, 0.000000000000000000, -8.000000000000000000 ) ) ;
#6820 = DIRECTION ( 'NONE',  ( -0.000000000000000000, -0.000000000000000000, -1.000000000000000000 ) ) ;
#6821 = DIRECTION ( 'NONE',  ( -1.000000000000000000, 0.000000000000000000, 0.000000000000000000 ) ) ;
#6822 = AXIS2_PLACEMENT_3D ( 'NONE', #13692, #13771, #14832 ) ;
#6823 = B_SPLINE_CURVE_WITH_KNOTS ( 'NONE', 3,
 ( #2161, #13486, #6779, #11363, #6483, #5364, #815, #897, #962, #9069 ),
 .UNSPECIFIED., .F., .F.,
 ( 4, 2, 2, 2, 4 ),
 ( 0.000000000000000000, 0.001708674401391109023, 0.003417348802782218045, 0.005126023204173327068, 0.006834697605564436090 ),
 .UNSPECIFIED. ) ;
#6824 = EDGE_CURVE ( 'NONE', #7767, #10678, #5025, .T. ) ;
#6825 = EDGE_LOOP ( 'NONE', ( #14028, #10727, #5178, #11515 ) ) ;
#6826 = CARTESIAN_POINT ( 'NONE',  ( 0.000000000000000000, 0.000000000000000000, -10.50000000000000000 ) ) ;
#6827 = EDGE_LOOP ( 'NONE', ( #7641, #10385, #3701, #5237 ) ) ;
#6828 = CYLINDRICAL_SURFACE ( 'NONE', #2526, 0.5000000000000073275 ) ;
#6829 = ADVANCED_FACE ( 'NONE', ( #12999 ), #2589, .T. ) ;
#6830 = CIRCLE ( 'NONE', #11473, 50.00000000000000000 ) ;
#6831 = ORIENTED_EDGE ( 'NONE', *, *, #3646, .T. ) ;
#6832 = B_SPLINE_CURVE_WITH_KNOTS ( 'NONE', 3,
 ( #5207, #11057, #5053, #6108, #495, #14311, #6183, #350, #3923, #12116, #8538, #14245, #658, #4148 ),
 .UNSPECIFIED., .F., .F.,
 ( 4, 2, 2, 2, 2, 2, 4 ),
 ( 0.000000000000000000, 0.001716022237784524482, 0.002574033356676786941, 0.003432044475569049399, 0.004290055594461312724, 0.005148066713353574748, 0.006864088951138102267 ),
 .UNSPECIFIED. ) ;
#6833 = CARTESIAN_POINT ( 'NONE',  ( -7.500000000000000888, 62.55197838597913318, 20.00000000000000000 ) ) ;
#6834 = DIRECTION ( 'NONE',  ( 1.000000000000000000, 0.000000000000000000, 0.000000000000000000 ) ) ;
#6835 = CARTESIAN_POINT ( 'NONE',  ( -97.00000000000000000, 1.015776140243522349E-12, -8.000000000000000000 ) ) ;
#6836 = DIRECTION ( 'NONE',  ( 1.000000000000000000, 0.000000000000000000, 0.000000000000000000 ) ) ;
#6837 = CARTESIAN_POINT ( 'NONE',  ( -4.203934362469272656, -1.640673743454848843, -3.598432614606966951 ) ) ;
#6838 = AXIS2_PLACEMENT_3D ( 'NONE', #4534, #12575, #11597 ) ;
#6839 = DIRECTION ( 'NONE',  ( 0.000000000000000000, 0.000000000000000000, -1.000000000000000000 ) ) ;
#6840 = ORIENTED_EDGE ( 'NONE', *, *, #8925, .F. ) ;
#6841 = VECTOR ( 'NONE', #8667, 1000.000000000000000 ) ;
#6842 = FACE_OUTER_BOUND ( 'NONE', #4619, .T. ) ;
#6843 = DIRECTION ( 'NONE',  ( 0.000000000000000000, 0.000000000000000000, 1.000000000000000000 ) ) ;
#6844 = EDGE_CURVE ( 'NONE', #8906, #4183, #9218, .T. ) ;
#6845 = EDGE_CURVE ( 'NONE', #2594, #8372, #12581, .T. ) ;
#6846 = FACE_OUTER_BOUND ( 'NONE', #6071, .T. ) ;
#6847 = DIRECTION ( 'NONE',  ( -1.000000000000000000, 0.000000000000000000, 0.000000000000000000 ) ) ;
#6848 = CIRCLE ( 'NONE', #9756, 53.55662432702593634 ) ;
#6849 = EDGE_LOOP ( 'NONE', ( #2577, #2413, #4660, #1439 ) ) ;
#6850 = CARTESIAN_POINT ( 'NONE',  ( -37.12029293941441210, -89.61631465359452875, -13.00000000000000178 ) ) ;
#6851 = VERTEX_POINT ( 'NONE', #8018 ) ;
#6852 = CIRCLE ( 'NONE', #5417, 2.500000000000000444 ) ;
#6853 = CARTESIAN_POINT ( 'NONE',  ( -12.50000000000000000, 61.74746958378133144, 15.00000000000000000 ) ) ;
#6854 = ADVANCED_FACE ( 'NONE', ( #11538 ), #12659, .F. ) ;
#6855 = CARTESIAN_POINT ( 'NONE',  ( -68.09867107463028901, -68.49330278050098286, -10.50000000000000000 ) ) ;
#6856 = DIRECTION ( 'NONE',  ( 0.000000000000000000, 0.000000000000000000, -1.000000000000000000 ) ) ;
#6857 = VERTEX_POINT ( 'NONE', #2881 ) ;
#6858 = ORIENTED_EDGE ( 'NONE', *, *, #4537, .T. ) ;
#6859 = VERTEX_POINT ( 'NONE', #617 ) ;
#6860 = DIRECTION ( 'NONE',  ( 0.000000000000000000, 0.000000000000000000, 1.000000000000000000 ) ) ;
#6861 = LINE ( 'NONE', #1182, #2053 ) ;
#6862 = EDGE_CURVE ( 'NONE', #14718, #13762, #10, .T. ) ;
#6863 =( REPRESENTATION_RELATIONSHIP ('NONE','NONE', #12187, #8100 ) REPRESENTATION_RELATIONSHIP_WITH_TRANSFORMATION ( #10059 )SHAPE_REPRESENTATION_RELATIONSHIP( ) );
#6864 = CARTESIAN_POINT ( 'NONE',  ( -3.999999999999996447, -0.3979232138631226268, 2.786738396466647721E-15 ) ) ;
#6865 = EDGE_LOOP ( 'NONE', ( #3916, #9371, #7326, #7618 ) ) ;
#6866 = VECTOR ( 'NONE', #2380, 1000.000000000000000 ) ;
#6867 = EDGE_LOOP ( 'NONE', ( #3158, #932, #4226, #2890, #11599, #683, #1324, #5372, #5214, #12034 ) ) ;
#6868 = ORIENTED_EDGE ( 'NONE', *, *, #14202, .F. ) ;
#6869 = CARTESIAN_POINT ( 'NONE',  ( 0.000000000000000000, 0.000000000000000000, -10.50000000000000000 ) ) ;
#6870 = DIRECTION ( 'NONE',  ( -0.000000000000000000, -0.000000000000000000, 1.000000000000000000 ) ) ;
#6871 = FACE_OUTER_BOUND ( 'NONE', #10546, .T. ) ;
#6872 = CIRCLE ( 'NONE', #340, 60.49999999999999289 ) ;
#6873 = CARTESIAN_POINT ( 'NONE',  ( -42.04772703543551415, -32.26435573746212526, -13.00000000000000178 ) ) ;
#6874 = AXIS2_PLACEMENT_3D ( 'NONE', #6452, #2977, #701 ) ;
#6875 = CIRCLE ( 'NONE', #5672, 3.000000000000002665 ) ;
#6876 = VERTEX_POINT ( 'NONE', #1130 ) ;
#6877 = DIRECTION ( 'NONE',  ( -1.000000000000000000, 0.000000000000000000, 0.000000000000000000 ) ) ;
#6878 = ORIENTED_EDGE ( 'NONE', *, *, #3525, .F. ) ;
#6879 = CARTESIAN_POINT ( 'NONE',  ( -68.58935777509570642, -68.58935777509452691, -10.50000000000000000 ) ) ;
#6880 = CARTESIAN_POINT ( 'NONE',  ( 44.79355920668812274, 31.05588327715851449, -13.00000000000000178 ) ) ;
#6881 = ORIENTED_EDGE ( 'NONE', *, *, #4866, .F. ) ;
#6882 = ORIENTED_EDGE ( 'NONE', *, *, #6741, .F. ) ;
#6883 = CIRCLE ( 'NONE', #7128, 53.55662432702593634 ) ;
#6884 = CARTESIAN_POINT ( 'NONE',  ( -22.05882352941176450, 71.68269180561142662, 23.50000000000000355 ) ) ;
#6885 = CIRCLE ( 'NONE', #4244, 0.5000000000000004441 ) ;
#6886 = AXIS2_PLACEMENT_3D ( 'NONE', #8162, #112, #6017 ) ;
#6887 = EDGE_CURVE ( 'NONE', #2976, #5777, #5822, .T. ) ;
#6888 = CIRCLE ( 'NONE', #11529, 53.55662432702593634 ) ;
#6889 = VERTEX_POINT ( 'NONE', #11302 ) ;
#6890 = EDGE_CURVE ( 'NONE', #14223, #11178, #8978, .T. ) ;
#6891 = DIRECTION ( 'NONE',  ( -1.000000000000000000, 0.000000000000000000, 0.000000000000000000 ) ) ;
#6892 = LINE ( 'NONE', #2121, #4899 ) ;
#6893 = DIRECTION ( 'NONE',  ( 0.000000000000000000, 0.000000000000000000, -1.000000000000000000 ) ) ;
#6894 = PLANE ( 'NONE',  #8005 ) ;
#6895 = AXIS2_PLACEMENT_3D ( 'NONE', #2486, #5896, #12818 ) ;
#6896 = CYLINDRICAL_SURFACE ( 'NONE', #13564, 2.649999999999985700 ) ;
#6897 = ORIENTED_EDGE ( 'NONE', *, *, #7210, .F. ) ;
#6898 = CIRCLE ( 'NONE', #10782, 3.000000000000004441 ) ;
#6899 = AXIS2_PLACEMENT_3D ( 'NONE', #3774, #2620, #7234 ) ;
#6900 = EDGE_CURVE ( 'NONE', #10355, #1483, #12155, .T. ) ;
#6901 = DIRECTION ( 'NONE',  ( 1.000000000000000000, 0.000000000000000000, 0.000000000000000000 ) ) ;
#6902 = CIRCLE ( 'NONE', #7631, 53.55662432702593634 ) ;
#6903 = CARTESIAN_POINT ( 'NONE',  ( -25.99999999999971223, -45.89934640057541060, 10.49999999999999822 ) ) ;
#6904 = ORIENTED_EDGE ( 'NONE', *, *, #6511, .T. ) ;
#6905 = EDGE_CURVE ( 'NONE', #7720, #12891, #5119, .T. ) ;
#6906 = DIRECTION ( 'NONE',  ( 0.000000000000000000, 0.000000000000000000, 1.000000000000000000 ) ) ;
#6907 = CIRCLE ( 'NONE', #4503, 2.649999999999985700 ) ;
#6908 = DIRECTION ( 'NONE',  ( -1.000000000000000000, 0.000000000000000000, 0.000000000000000000 ) ) ;
#6909 = ADVANCED_FACE ( 'NONE', ( #6718 ), #6356, .F. ) ;
#6910 = CARTESIAN_POINT ( 'NONE',  ( -10.87743925404099699, 62.05426862177564118, 18.69798886497097357 ) ) ;
#6911 = CIRCLE ( 'NONE', #9096, 52.50000000000000711 ) ;
#6912 = CARTESIAN_POINT ( 'NONE',  ( -45.88839665196098849, 26.99988008862674960, -13.00000000000000178 ) ) ;
#6913 = CARTESIAN_POINT ( 'NONE',  ( 0.000000000000000000, 0.000000000000000000, -8.000000000000000000 ) ) ;
#6914 = CARTESIAN_POINT ( 'NONE',  ( -29.26435573746199381, 42.04772703543562073, 8.000000000000000000 ) ) ;
#6915 = FACE_OUTER_BOUND ( 'NONE', #10640, .T. ) ;
#6916 = AXIS2_PLACEMENT_3D ( 'NONE', #6558, #9904, #11212 ) ;
#6917 = DIRECTION ( 'NONE',  ( -0.000000000000000000, -0.000000000000000000, -1.000000000000000000 ) ) ;
#6918 = AXIS2_PLACEMENT_3D ( 'NONE', #10552, #221, #9623 ) ;
#6919 = ORIENTED_EDGE ( 'NONE', *, *, #530, .F. ) ;
#6920 = PLANE ( 'NONE',  #10341 ) ;
#6921 = CARTESIAN_POINT ( 'NONE',  ( 26.01438936481372721, 47.21331623427104063, 10.49999999999999822 ) ) ;
#6922 = CARTESIAN_POINT ( 'NONE',  ( -10.71740939043329099, 51.19406879332069593, 8.000000000000000000 ) ) ;
#6923 = CARTESIAN_POINT ( 'NONE',  ( 0.000000000000000000, 0.000000000000000000, 8.000000000000000000 ) ) ;
#6924 = EDGE_LOOP ( 'NONE', ( #10173, #5484, #10064, #10441 ) ) ;
#6925 = CYLINDRICAL_SURFACE ( 'NONE', #13366, 0.5000000000000073275 ) ;
#6926 = ORIENTED_EDGE ( 'NONE', *, *, #321, .T. ) ;
#6927 = CARTESIAN_POINT ( 'NONE',  ( -25.00000000000000000, 81.24038404635962252, -31.00000000000000000 ) ) ;
#6928 = CARTESIAN_POINT ( 'NONE',  ( -3.999999999999995559, 0.7924765000094611267, -0.05906175389889475880 ) ) ;
#6929 = EDGE_CURVE ( 'NONE', #2714, #7912, #10444, .T. ) ;
#6930 = DIRECTION ( 'NONE',  ( 1.000000000000000000, 1.765157221169382931E-15, 0.000000000000000000 ) ) ;
#6931 = ADVANCED_FACE ( 'NONE', ( #14430, #8645 ), #9082, .T. ) ;
#6932 = DIRECTION ( 'NONE',  ( -0.000000000000000000, -0.000000000000000000, 1.000000000000000000 ) ) ;
#6933 = ORIENTED_EDGE ( 'NONE', *, *, #5369, .F. ) ;
#6934 = CIRCLE ( 'NONE', #1384, 0.5000000000000004441 ) ;
#6935 = ORIENTED_EDGE ( 'NONE', *, *, #321, .F. ) ;
#6936 = VECTOR ( 'NONE', #3142, 1000.000000000000000 ) ;
#6937 = CARTESIAN_POINT ( 'NONE',  ( 90.11631465359468507, -37.12029293941410657, 10.49999999999999822 ) ) ;
#6938 = CARTESIAN_POINT ( 'NONE',  ( 97.00000000000000000, -3.384287605079545030E-13, 8.000000000000000000 ) ) ;
#6939 = CYLINDRICAL_SURFACE ( 'NONE', #59, 50.00000000000000000 ) ;
#6940 = EDGE_LOOP ( 'NONE', ( #11935, #1456, #13044, #190, #11643 ) ) ;
#6941 = ADVANCED_FACE ( 'NONE', ( #5245 ), #4542, .T. ) ;
#6942 = B_SPLINE_CURVE_WITH_KNOTS ( 'NONE', 3,
 ( #13426, #13500, #4251, #2036, #754, #9847, #3104, #13566, #11309, #3031, #6494, #2948, #10998, #10003, #8866, #14729, #831, #911, #7717, #5528 ),
 .UNSPECIFIED., .F., .F.,
 ( 4, 2, 2, 2, 2, 2, 2, 2, 2, 4 ),
 ( 0.000000000000000000, 0.0009815662899613972463, 0.001472349434942093376, 0.001963132579922789289, 0.002944698869884177211, 0.003926265159845564699, 0.004907831449806952621, 0.005889397739768340544, 0.006870964029729727598, 0.007852530319691115521 ),
 .UNSPECIFIED. ) ;
#6943 = ORIENTED_EDGE ( 'NONE', *, *, #11550, .F. ) ;
#6944 = ORIENTED_EDGE ( 'NONE', *, *, #10831, .F. ) ;
#6945 = CARTESIAN_POINT ( 'NONE',  ( -25.00000000000000000, 81.24038404635962252, 26.00000000000000000 ) ) ;
#6946 = DIRECTION ( 'NONE',  ( 0.000000000000000000, 0.000000000000000000, 1.000000000000000000 ) ) ;
#6947 = EDGE_CURVE ( 'NONE', #13983, #14637, #1052, .T. ) ;
#6948 = CARTESIAN_POINT ( 'NONE',  ( 2.500000000000002220, 0.000000000000000000, 0.000000000000000000 ) ) ;
#6949 =( NAMED_UNIT ( * ) PLANE_ANGLE_UNIT ( ) SI_UNIT ( $, .RADIAN. ) );
#6950 = CARTESIAN_POINT ( 'NONE',  ( -37.12029293941441210, -89.61631465359452875, -13.00000000000000178 ) ) ;
#6951 = ORIENTED_EDGE ( 'NONE', *, *, #6263, .T. ) ;
#6952 = DIRECTION ( 'NONE',  ( 1.000000000000000000, 0.000000000000000000, 0.000000000000000000 ) ) ;
#6953 = ORIENTED_EDGE ( 'NONE', *, *, #10812, .F. ) ;
#6954 = DIRECTION ( 'NONE',  ( 0.000000000000000000, 0.000000000000000000, 1.000000000000000000 ) ) ;
#6955 = CARTESIAN_POINT ( 'NONE',  ( 37.02125851216354846, -90.10640870805738700, 10.49999999999999822 ) ) ;
#6956 = EDGE_LOOP ( 'NONE', ( #3660, #282, #13658, #12189 ) ) ;
#6957 = ORIENTED_EDGE ( 'NONE', *, *, #2721, .T. ) ;
#6958 = CARTESIAN_POINT ( 'NONE',  ( 13.35619814848834075, -51.53979475227123430, -13.00000000000000178 ) ) ;
#6959 = ORIENTED_EDGE ( 'NONE', *, *, #9036, .F. ) ;
#6960 = FACE_BOUND ( 'NONE', #300, .T. ) ;
#6961 = DIRECTION ( 'NONE',  ( 0.000000000000000000, -0.5000000000000012212, -0.8660254037844380415 ) ) ;
#6962 = CARTESIAN_POINT ( 'NONE',  ( -1.317756351988341290, 3.857995168970199895, -0.04852650426601234218 ) ) ;
#6963 = CARTESIAN_POINT ( 'NONE',  ( -3.522875095019435854, 2.820352903225096686, -3.598441714920458612 ) ) ;
#6964 = EDGE_LOOP ( 'NONE', ( #692, #8791 ) ) ;
#6965 = DIRECTION ( 'NONE',  ( 0.000000000000000000, 0.000000000000000000, 1.000000000000000000 ) ) ;
#6966 = ORIENTED_EDGE ( 'NONE', *, *, #8762, .F. ) ;
#6967 =( LENGTH_UNIT ( ) NAMED_UNIT ( * ) SI_UNIT ( .MILLI., .METRE. ) );
#6968 = APPLICATION_CONTEXT ( 'automotive_design' ) ;
#6969 = ADVANCED_FACE ( 'NONE', ( #8716 ), #9155, .F. ) ;
#6970 = DIRECTION ( 'NONE',  ( -1.000000000000000000, 0.000000000000000000, 0.000000000000000000 ) ) ;
#6971 = EDGE_CURVE ( 'NONE', #13693, #6509, #10210, .T. ) ;
#6972 = ORIENTED_EDGE ( 'NONE', *, *, #3939, .F. ) ;
#6973 = VERTEX_POINT ( 'NONE', #13645 ) ;
#6974 = CARTESIAN_POINT ( 'NONE',  ( 29.95643228365060295, 96.45524571768993383, 12.60642518152332769 ) ) ;
#6975 = ORIENTED_EDGE ( 'NONE', *, *, #4723, .T. ) ;
#6976 = DIRECTION ( 'NONE',  ( 0.000000000000000000, 0.000000000000000000, -1.000000000000000000 ) ) ;
#6977 = DIRECTION ( 'NONE',  ( -0.000000000000000000, -0.000000000000000000, -1.000000000000000000 ) ) ;
#6978 = CARTESIAN_POINT ( 'NONE',  ( 22.05882352941176094, 71.68269180561141241, 13.50000000000000533 ) ) ;
#6979 = CARTESIAN_POINT ( 'NONE',  ( 5.200000000000006395, 0.000000000000000000, 2.500000000000028422 ) ) ;
#6980 = FACE_OUTER_BOUND ( 'NONE', #14173, .T. ) ;
#6981 = CARTESIAN_POINT ( 'NONE',  ( 32.26435573746228158, -42.04772703543541468, -8.000000000000000000 ) ) ;
#6982 = ORIENTED_EDGE ( 'NONE', *, *, #3838, .F. ) ;
#6983 = EDGE_CURVE ( 'NONE', #9441, #13119, #2692, .T. ) ;
#6984 = ADVANCED_FACE ( 'NONE', ( #274, #1267 ), #1190, .T. ) ;
#6985 = DIRECTION ( 'NONE',  ( 1.000000000000000000, 0.000000000000000000, 0.000000000000000000 ) ) ;
#6986 = DIRECTION ( 'NONE',  ( 0.000000000000000000, 0.000000000000000000, 1.000000000000000000 ) ) ;
#6987 = CYLINDRICAL_SURFACE ( 'NONE', #5160, 63.00000000000000000 ) ;
#6988 = CARTESIAN_POINT ( 'NONE',  ( -3.492805317593278058, 46.55633131742322917, -10.50000000000000000 ) ) ;
#6989 = ORIENTED_EDGE ( 'NONE', *, *, #8091, .T. ) ;
#6990 = DIRECTION ( 'NONE',  ( 0.000000000000000000, 0.000000000000000000, 1.000000000000000000 ) ) ;
#6991 = ORIENTED_EDGE ( 'NONE', *, *, #4069, .F. ) ;
#6992 = LINE ( 'NONE', #6853, #13828 ) ;
#6993 = CARTESIAN_POINT ( 'NONE',  ( -3.999999999999996447, 2.309401076758498039, -0.4999999999999935052 ) ) ;
#6994 = VECTOR ( 'NONE', #3817, 1000.000000000000000 ) ;
#6995 = CARTESIAN_POINT ( 'NONE',  ( 0.000000000000000000, 0.000000000000000000, 23.50000000000000355 ) ) ;
#6996 = CARTESIAN_POINT ( 'NONE',  ( 0.000000000000000000, 0.000000000000000000, -10.50000000000000000 ) ) ;
#6997 = ORIENTED_EDGE ( 'NONE', *, *, #12618, .T. ) ;
#6998 = ORIENTED_EDGE ( 'NONE', *, *, #3671, .T. ) ;
#6999 = CARTESIAN_POINT ( 'NONE',  ( -9.717538815323484513, 62.24844358264333266, -19.51802576651051879 ) ) ;
#7000 = AXIS2_PLACEMENT_3D ( 'NONE', #8685, #14394, #13262 ) ;
#7001 = DIRECTION ( 'NONE',  ( -0.000000000000000000, -0.000000000000000000, -1.000000000000000000 ) ) ;
#7002 = DIRECTION ( 'NONE',  ( 0.2941176470588238168, -0.9557692240748187906, 0.000000000000000000 ) ) ;
#7003 = ORIENTED_EDGE ( 'NONE', *, *, #14510, .T. ) ;
#7004 = VECTOR ( 'NONE', #12232, 1000.000000000000000 ) ;
#7005 = ADVANCED_FACE ( 'NONE', ( #12878 ), #2444, .F. ) ;
#7006 = EDGE_LOOP ( 'NONE', ( #7543, #1520, #6671, #13297, #1805, #13660 ) ) ;
#7007 = ORIENTED_EDGE ( 'NONE', *, *, #9123, .T. ) ;
#7008 = EDGE_CURVE ( 'NONE', #1677, #10850, #12643, .T. ) ;
#7009 = CARTESIAN_POINT ( 'NONE',  ( 0.000000000000000000, 0.000000000000000000, -10.50000000000000000 ) ) ;
#7010 = CIRCLE ( 'NONE', #12365, 56.99999999999999289 ) ;
#7011 = CARTESIAN_POINT ( 'NONE',  ( 2.756197834950067538, 3.027510591568720599, -3.223146290109807133 ) ) ;
#7012 = CIRCLE ( 'NONE', #12133, 2.041999999999999815 ) ;
#7013 = DIRECTION ( 'NONE',  ( 0.000000000000000000, 0.000000000000000000, 1.000000000000000000 ) ) ;
#7014 = EDGE_CURVE ( 'NONE', #11546, #9586, #14092, .T. ) ;
#7015 = AXIS2_PLACEMENT_3D ( 'NONE', #28, #5649, #103 ) ;
#7016 = VERTEX_POINT ( 'NONE', #7090 ) ;
#7017 = CARTESIAN_POINT ( 'NONE',  ( 4.121772567811984089, 51.45950017607689375, -8.000000000000000000 ) ) ;
#7018 = EDGE_LOOP ( 'NONE', ( #3934, #7425, #11379, #10122, #2175, #3243, #5797, #1419, #2476, #1817, #5985 ) ) ;
#7019 = AXIS2_PLACEMENT_3D ( 'NONE', #9631, #6142, #2816 ) ;
#7020 = CARTESIAN_POINT ( 'NONE',  ( -23.49999999999971223, -45.89934640057541060, -8.000000000000000000 ) ) ;
#7021 = LINE ( 'NONE', #12965, #14500 ) ;
#7022 = ORIENTED_EDGE ( 'NONE', *, *, #2823, .F. ) ;
#7023 = EDGE_CURVE ( 'NONE', #3583, #12891, #8169, .T. ) ;
#7024 = VECTOR ( 'NONE', #14977, 1000.000000000000000 ) ;
#7025 = EDGE_CURVE ( 'NONE', #12545, #4523, #8991, .T. ) ;
#7026 = VERTEX_POINT ( 'NONE', #5803 ) ;
#7027 = DIRECTION ( 'NONE',  ( -0.000000000000000000, -0.000000000000000000, 1.000000000000000000 ) ) ;
#7028 = AXIS2_PLACEMENT_3D ( 'NONE', #3737, #3881, #3957 ) ;
#7029 = VERTEX_POINT ( 'NONE', #11896 ) ;
#7030 = CARTESIAN_POINT ( 'NONE',  ( 0.000000000000000000, 0.000000000000000000, -8.000000000000000000 ) ) ;
#7031 = DIRECTION ( 'NONE',  ( 1.000000000000000000, 0.000000000000000000, 0.000000000000000000 ) ) ;
#7032 = CARTESIAN_POINT ( 'NONE',  ( 0.000000000000000000, 0.000000000000000000, -8.000000000000000000 ) ) ;
#7033 = CARTESIAN_POINT ( 'NONE',  ( -0.6640947660594231916, 4.471078309994339861, -3.602146406945769819 ) ) ;
#7034 = EDGE_CURVE ( 'NONE', #12827, #1689, #9375, .T. ) ;
#7035 = MECHANICAL_DESIGN_GEOMETRIC_PRESENTATION_REPRESENTATION (  '', ( #1473 ), #6100 ) ;
#7036 = ORIENTED_EDGE ( 'NONE', *, *, #4326, .T. ) ;
#7038 = CIRCLE ( 'NONE', #758, 3.000000000000002665 ) ;
#7037 = DIRECTION ( 'NONE',  ( 0.000000000000000000, 0.000000000000000000, 1.000000000000000000 ) ) ;
#7039 = DIRECTION ( 'NONE',  ( 0.000000000000000000, 0.000000000000000000, 1.000000000000000000 ) ) ;
#7040 = EDGE_LOOP ( 'NONE', ( #2730, #5504, #4011, #12862 ) ) ;
#7041 = AXIS2_PLACEMENT_3D ( 'NONE', #9859, #11453, #14502 ) ;
#7042 = DIRECTION ( 'NONE',  ( 0.000000000000000000, 0.000000000000000000, 1.000000000000000000 ) ) ;
#7043 = CIRCLE ( 'NONE', #4404, 0.5000000000000004441 ) ;
#7044 = VERTEX_POINT ( 'NONE', #1346 ) ;
#7045 = CARTESIAN_POINT ( 'NONE',  ( 9.706953719245472456, 57.06275842387054098, -10.50000000000000000 ) ) ;
#7046 = ORIENTED_EDGE ( 'NONE', *, *, #9431, .F. ) ;
#7047 = AXIS2_PLACEMENT_3D ( 'NONE', #5809, #12811, #11542 ) ;
#7048 = CARTESIAN_POINT ( 'NONE',  ( 38.26834323650837888, -92.38795325112893408, 8.000000000000000000 ) ) ;
#7049 = ORIENTED_EDGE ( 'NONE', *, *, #13360, .T. ) ;
#7050 = FACE_OUTER_BOUND ( 'NONE', #5193, .T. ) ;
#7051 = AXIS2_PLACEMENT_3D ( 'NONE', #12596, #2047, #2193 ) ;
#7052 = DIRECTION ( 'NONE',  ( 0.000000000000000000, 0.000000000000000000, 1.000000000000000000 ) ) ;
#7053 = DIRECTION ( 'NONE',  ( -1.000000000000000000, 0.000000000000000000, 0.000000000000000000 ) ) ;
#7054 = CYLINDRICAL_SURFACE ( 'NONE', #10657, 2.649999999999985700 ) ;
#7055 = CYLINDRICAL_SURFACE ( 'NONE', #6505, 60.50000000000000711 ) ;
#7056 = PRODUCT_CONTEXT ( 'NONE', #674, 'mechanical' ) ;
#7057 = CARTESIAN_POINT ( 'NONE',  ( 45.96504489226007450, -23.50071946824056823, -8.000000000000000000 ) ) ;
#7058 = MECHANICAL_DESIGN_GEOMETRIC_PRESENTATION_REPRESENTATION (  '', ( #11202 ), #529 ) ;
#7059 = EDGE_LOOP ( 'NONE', ( #5028, #6006, #9066 ) ) ;
#7060 = CARTESIAN_POINT ( 'NONE',  ( 0.2790467552932217044, -96.58511096861892042, -13.00000000000000178 ) ) ;
#7061 = CARTESIAN_POINT ( 'NONE',  ( -2.000000000000008882, -3.464101615137750390, 0.000000000000000000 ) ) ;
#7062 = VECTOR ( 'NONE', #4412, 1000.000000000000000 ) ;
#7063 = FACE_OUTER_BOUND ( 'NONE', #2115, .T. ) ;
#7064 = LINE ( 'NONE', #12559, #7841 ) ;
#7065 = ORIENTED_EDGE ( 'NONE', *, *, #73, .T. ) ;
#7066 = EDGE_CURVE ( 'NONE', #7077, #13418, #3551, .T. ) ;
#7067 = CYLINDRICAL_SURFACE ( 'NONE', #1257, 52.50000000000000711 ) ;
#7068 = EDGE_LOOP ( 'NONE', ( #10474, #1866, #6566, #1086 ) ) ;
#7069 = AXIS2_PLACEMENT_3D ( 'NONE', #5950, #12107, #14159 ) ;
#7070 = EDGE_CURVE ( 'NONE', #1683, #3137, #2554, .T. ) ;
#7071 = CYLINDRICAL_SURFACE ( 'NONE', #12370, 3.000000000000002665 ) ;
#7072 = EDGE_CURVE ( 'NONE', #10615, #4717, #4685, .T. ) ;
#7073 = EDGE_CURVE ( 'NONE', #10743, #7688, #7293, .T. ) ;
#7074 = CYLINDRICAL_SURFACE ( 'NONE', #10459, 3.000000000000002665 ) ;
#7075 = DIRECTION ( 'NONE',  ( -1.000000000000000000, 0.000000000000000000, 0.000000000000000000 ) ) ;
#7076 = ORIENTED_EDGE ( 'NONE', *, *, #694, .F. ) ;
#7077 = VERTEX_POINT ( 'NONE', #13033 ) ;
#7078 = DIRECTION ( 'NONE',  ( 0.000000000000000000, 0.000000000000000000, -1.000000000000000000 ) ) ;
#7079 = CARTESIAN_POINT ( 'NONE',  ( 45.46633369868310837, -26.24999999999987921, -10.50000000000000000 ) ) ;
#7080 = AXIS2_PLACEMENT_3D ( 'NONE', #4471, #12809, #5670 ) ;
#7081 = AXIS2_PLACEMENT_3D ( 'NONE', #4295, #5345, #10120 ) ;
#7082 = DIRECTION ( 'NONE',  ( 1.000000000000000000, 0.000000000000000000, 0.000000000000000000 ) ) ;
#7083 = ORIENTED_EDGE ( 'NONE', *, *, #444, .T. ) ;
#7084 = VERTEX_POINT ( 'NONE', #2392 ) ;
#7085 = CIRCLE ( 'NONE', #13915, 100.0000000000000000 ) ;
#7086 = EDGE_LOOP ( 'NONE', ( #4, #8691, #14482, #11683 ) ) ;
#7087 = ADVANCED_FACE ( 'NONE', ( #122 ), #14166, .T. ) ;
#7088 = FACE_OUTER_BOUND ( 'NONE', #12869, .T. ) ;
#7089 = VECTOR ( 'NONE', #10167, 1000.000000000000000 ) ;
#7090 = CARTESIAN_POINT ( 'NONE',  ( 9.154234823626464946E-15, 100.0000000000000000, -8.000000000000000000 ) ) ;
#7091 = DIRECTION ( 'NONE',  ( 0.000000000000000000, 0.000000000000000000, 1.000000000000000000 ) ) ;
#7092 = CARTESIAN_POINT ( 'NONE',  ( -13.60620885621536935, 51.79945067148138094, -10.50000000000000000 ) ) ;
#7093 = CARTESIAN_POINT ( 'NONE',  ( -2.449293598294708880E-16, 38.00000000000000000, -28.00000000000000000 ) ) ;
#7094 = ADVANCED_FACE ( 'NONE', ( #4827 ), #5956, .T. ) ;
#7095 = ORIENTED_EDGE ( 'NONE', *, *, #12158, .T. ) ;
#7096 = CARTESIAN_POINT ( 'NONE',  ( 2.500000000000002220, 0.000000000000000000, 0.000000000000000000 ) ) ;
#7097 = CARTESIAN_POINT ( 'NONE',  ( 0.000000000000000000, 0.000000000000000000, -16.00000000000000000 ) ) ;
#7098 = AXIS2_PLACEMENT_3D ( 'NONE', #12794, #3538, #5653 ) ;
#7099 = DIRECTION ( 'NONE',  ( 0.000000000000000000, 0.000000000000000000, 1.000000000000000000 ) ) ;
#7100 = ORIENTED_EDGE ( 'NONE', *, *, #13393, .T. ) ;
#7101 = CIRCLE ( 'NONE', #574, 63.00000000000000000 ) ;
#7102 = ORIENTED_EDGE ( 'NONE', *, *, #3186, .F. ) ;
#7103 = CARTESIAN_POINT ( 'NONE',  ( 19.68583958711426263, -30.74264578624780597, -25.50000000000000355 ) ) ;
#7104 = ORIENTED_EDGE ( 'NONE', *, *, #10575, .F. ) ;
#7105 = VECTOR ( 'NONE', #8293, 1000.000000000000114 ) ;
#7106 = AXIS2_PLACEMENT_3D ( 'NONE', #5514, #12349, #14778 ) ;
#7107 = CARTESIAN_POINT ( 'NONE',  ( -25.00000000000000000, 81.24038404635962252, -23.50000000000000000 ) ) ;
#7108 = DIRECTION ( 'NONE',  ( 1.000000000000000000, 0.000000000000000000, 0.000000000000000000 ) ) ;
#7109 = AXIS2_PLACEMENT_3D ( 'NONE', #14757, #14042, #7113 ) ;
#7110 = CARTESIAN_POINT ( 'NONE',  ( 0.000000000000000000, -1.178949249685222522, -2.042000000000002036 ) ) ;
#7111 = CARTESIAN_POINT ( 'NONE',  ( -44.79355920668832880, -31.05588327715819474, -13.00000000000000178 ) ) ;
#7112 = EDGE_CURVE ( 'NONE', #5604, #3464, #9474, .T. ) ;
#7113 = DIRECTION ( 'NONE',  ( -1.000000000000000000, 0.000000000000000000, 0.000000000000000000 ) ) ;
#7114 = DIRECTION ( 'NONE',  ( 0.000000000000000000, 0.000000000000000000, -1.000000000000000000 ) ) ;
#7115 = EDGE_CURVE ( 'NONE', #3630, #9614, #10695, .T. ) ;
#7116 = ORIENTED_EDGE ( 'NONE', *, *, #13743, .F. ) ;
#7117 = DIRECTION ( 'NONE',  ( -1.000000000000000000, 0.000000000000000000, 0.000000000000000000 ) ) ;
#7118 = EDGE_CURVE ( 'NONE', #2051, #345, #4888, .T. ) ;
#7119 = AXIS2_PLACEMENT_3D ( 'NONE', #14988, #13774, #8290 ) ;
#7120 = VECTOR ( 'NONE', #6569, 1000.000000000000000 ) ;
#7121 = ORIENTED_EDGE ( 'NONE', *, *, #10237, .F. ) ;
#7122 = SURFACE_STYLE_USAGE ( .BOTH. , #4864 ) ;
#7123 = EDGE_CURVE ( 'NONE', #7242, #6515, #8751, .T. ) ;
#7124 = DIRECTION ( 'NONE',  ( -1.000000000000000000, 0.000000000000000000, 0.000000000000000000 ) ) ;
#7125 = ORIENTED_EDGE ( 'NONE', *, *, #266, .T. ) ;
#7126 = DIRECTION ( 'NONE',  ( 1.000000000000000000, -1.765157221169382931E-15, 0.000000000000000000 ) ) ;
#7127 = AXIS2_PLACEMENT_3D ( 'NONE', #4742, #4442, #1240 ) ;
#7128 = AXIS2_PLACEMENT_3D ( 'NONE', #14319, #6254, #3931 ) ;
#7129 = FACE_OUTER_BOUND ( 'NONE', #4492, .T. ) ;
#7130 = DIRECTION ( 'NONE',  ( 1.000000000000000000, 0.000000000000000000, 0.000000000000000000 ) ) ;
#7131 = CARTESIAN_POINT ( 'NONE',  ( 13.71740939043365337, -51.19406879332061067, -8.000000000000000000 ) ) ;
#7132 = AXIS2_PLACEMENT_3D ( 'NONE', #5137, #430, #5968 ) ;
#7133 = CIRCLE ( 'NONE', #4496, 63.00000000000000000 ) ;
#7134 = CARTESIAN_POINT ( 'NONE',  ( -4.197312064133470244, -0.8182229787989945269, -3.502518405183887573 ) ) ;
#7135 = ITEM_DEFINED_TRANSFORMATION ( 'NONE', 'NONE', #9915,  #5108 ) ;
#7136 = ADVANCED_FACE ( 'NONE', ( #7625 ), #4165, .T. ) ;
#7137 = EDGE_LOOP ( 'NONE', ( #3254, #953, #13048, #11096 ) ) ;
#7138 = CARTESIAN_POINT ( 'NONE',  ( -15.88467684210512942, 49.11971303961693280, -8.000000000000000000 ) ) ;
#7139 = ORIENTED_EDGE ( 'NONE', *, *, #700, .F. ) ;
#7140 = CARTESIAN_POINT ( 'NONE',  ( 1.144235203016665592, 3.958177651039090250, -0.09382832055445507191 ) ) ;
#7141 = DIRECTION ( 'NONE',  ( 1.000000000000000000, 0.000000000000000000, 0.000000000000000000 ) ) ;
#7142 = CIRCLE ( 'NONE', #3772, 5.000000000000001776 ) ;
#7143 = DIRECTION ( 'NONE',  ( -0.000000000000000000, -0.000000000000000000, -1.000000000000000000 ) ) ;
#7144 = CIRCLE ( 'NONE', #12985, 3.000000000000002665 ) ;
#7145 = AXIS2_PLACEMENT_3D ( 'NONE', #14039, #5904, #148 ) ;
#7146 = CARTESIAN_POINT ( 'NONE',  ( -4.121772567811602173, -51.45950017607692217, 8.000000000000000000 ) ) ;
#7147 = VERTEX_POINT ( 'NONE', #9826 ) ;
#7148 = DIRECTION ( 'NONE',  ( -1.000000000000000000, 0.000000000000000000, 0.000000000000000000 ) ) ;
#7149 = VERTEX_POINT ( 'NONE', #9743 ) ;
#7150 = ORIENTED_EDGE ( 'NONE', *, *, #3112, .T. ) ;
#7151 = CARTESIAN_POINT ( 'NONE',  ( -6.917888187662729393, -52.54657765281195481, 8.000000000000000000 ) ) ;
#7152 = DIRECTION ( 'NONE',  ( 1.000000000000000000, 0.000000000000000000, 0.000000000000000000 ) ) ;
#7153 = VECTOR ( 'NONE', #7321, 1000.000000000000000 ) ;
#7154 = AXIS2_PLACEMENT_3D ( 'NONE', #2271, #11549, #10236 ) ;
#7155 = DIRECTION ( 'NONE',  ( 1.000000000000000000, 0.000000000000000000, 0.000000000000000000 ) ) ;
#7156 = CARTESIAN_POINT ( 'NONE',  ( -92.55687898036933348, -36.52608637591544039, -8.000000000000000000 ) ) ;
#7157 = ORIENTED_EDGE ( 'NONE', *, *, #10151, .T. ) ;
#7158 = VERTEX_POINT ( 'NONE', #12194 ) ;
#7159 = DIRECTION ( 'NONE',  ( 1.000000000000000000, 0.000000000000000000, 0.000000000000000000 ) ) ;
#7160 = DIRECTION ( 'NONE',  ( 0.000000000000000000, 0.000000000000000000, 1.000000000000000000 ) ) ;
#7161 = CARTESIAN_POINT ( 'NONE',  ( 0.000000000000000000, 0.000000000000000000, -16.00000000000000000 ) ) ;
#7162 = EDGE_CURVE ( 'NONE', #13279, #4787, #20, .T. ) ;
#7163 = AXIS2_PLACEMENT_3D ( 'NONE', #5886, #14026, #8171 ) ;
#7164 = ORIENTED_EDGE ( 'NONE', *, *, #12941, .F. ) ;
#7165 = EDGE_CURVE ( 'NONE', #14898, #7167, #3912, .T. ) ;
#7166 = EDGE_LOOP ( 'NONE', ( #11121, #7076, #6119, #5146, #1058 ) ) ;
#7167 = VERTEX_POINT ( 'NONE', #7319 ) ;
#7168 = CARTESIAN_POINT ( 'NONE',  ( 18.52941176470587692, 60.21346111671358159, -26.00000000000000000 ) ) ;
#7169 = CARTESIAN_POINT ( 'NONE',  ( 89.61631465359491244, 37.12029293941346708, 8.000000000000000000 ) ) ;
#7170 = PLANE ( 'NONE',  #2495 ) ;
#7171 =( NAMED_UNIT ( * ) SI_UNIT ( $, .STERADIAN. ) SOLID_ANGLE_UNIT ( ) );
#7172 = CARTESIAN_POINT ( 'NONE',  ( 2.649999999999988809, 38.00000000000000000, -25.50000000000000355 ) ) ;
#7173 = AXIS2_PLACEMENT_3D ( 'NONE', #9292, #10214, #1120 ) ;
#7174 = ORIENTED_EDGE ( 'NONE', *, *, #2677, .T. ) ;
#7175 = EDGE_LOOP ( 'NONE', ( #12366, #12078, #14767, #14493, #8269, #12749, #183 ) ) ;
#7176 = DIRECTION ( 'NONE',  ( -1.000000000000000000, 0.000000000000000000, 0.000000000000000000 ) ) ;
#7177 = CARTESIAN_POINT ( 'NONE',  ( -51.19406879332065330, -13.71740939043347041, -8.000000000000000000 ) ) ;
#7178 = CARTESIAN_POINT ( 'NONE',  ( -9.706953719245875689, -57.06275842387046993, -10.50000000000000000 ) ) ;
#7179 = VECTOR ( 'NONE', #13563, 1000.000000000000000 ) ;
#7180 = EDGE_CURVE ( 'NONE', #3301, #6492, #2925, .T. ) ;
#7181 = ORIENTED_EDGE ( 'NONE', *, *, #5724, .T. ) ;
#7182 = VERTEX_POINT ( 'NONE', #2851 ) ;
#7183 = CARTESIAN_POINT ( 'NONE',  ( -49.11971303961688307, -15.88467684210530528, -13.00000000000000178 ) ) ;
#7184 = AXIS2_PLACEMENT_3D ( 'NONE', #2145, #14987, #12782 ) ;
#7185 = ORIENTED_EDGE ( 'NONE', *, *, #42, .T. ) ;
#7186 = DIRECTION ( 'NONE',  ( 0.000000000000000000, 0.000000000000000000, 1.000000000000000000 ) ) ;
#7187 = DIRECTION ( 'NONE',  ( 0.000000000000000000, 0.000000000000000000, -1.000000000000000000 ) ) ;
#7188 = CARTESIAN_POINT ( 'NONE',  ( -3.999999999999996447, -2.309401076758512250, -3.504269196027871569 ) ) ;
#7189 = DIRECTION ( 'NONE',  ( 0.000000000000000000, 0.000000000000000000, 1.000000000000000000 ) ) ;
#7190 = ORIENTED_EDGE ( 'NONE', *, *, #10884, .T. ) ;
#7191 = CARTESIAN_POINT ( 'NONE',  ( -11.08463629228402603, 74.17659209477393745, -18.49742775384897442 ) ) ;
#7192 = CARTESIAN_POINT ( 'NONE',  ( -71.53347797788821083, -69.16568774265570596, 8.000000000000000000 ) ) ;
#7193 = ORIENTED_EDGE ( 'NONE', *, *, #2763, .T. ) ;
#7194 = DIRECTION ( 'NONE',  ( 1.000000000000000000, 0.000000000000000000, 0.000000000000000000 ) ) ;
#7195 = ORIENTED_EDGE ( 'NONE', *, *, #6354, .T. ) ;
#7196 = VERTEX_POINT ( 'NONE', #3001 ) ;
#7197 = PRESENTATION_STYLE_ASSIGNMENT (( #7122 ) ) ;
#7198 = EDGE_CURVE ( 'NONE', #12633, #5385, #7281, .T. ) ;
#7199 = EDGE_LOOP ( 'NONE', ( #14968, #12518, #5399, #8127 ) ) ;
#7200 = EDGE_CURVE ( 'NONE', #8562, #2510, #13121, .T. ) ;
#7201 = CARTESIAN_POINT ( 'NONE',  ( 49.00442420935993226, -30.80502811811213704, 8.000000000000000000 ) ) ;
#7202 = EDGE_CURVE ( 'NONE', #6323, #5248, #1963, .T. ) ;
#7203 = CARTESIAN_POINT ( 'NONE',  ( 9.706953719245472456, 57.06275842387054098, -8.000000000000000000 ) ) ;
#7204 = CIRCLE ( 'NONE', #3833, 100.0000000000000000 ) ;
#7205 = DIRECTION ( 'NONE',  ( -1.000000000000000000, 0.000000000000000000, 0.000000000000000000 ) ) ;
#7206 = DIRECTION ( 'NONE',  ( -0.000000000000000000, -0.000000000000000000, -1.000000000000000000 ) ) ;
#7207 = FACE_OUTER_BOUND ( 'NONE', #12076, .T. ) ;
#7208 = FACE_OUTER_BOUND ( 'NONE', #401, .T. ) ;
#7209 = ORIENTED_EDGE ( 'NONE', *, *, #8944, .F. ) ;
#7210 = EDGE_CURVE ( 'NONE', #4832, #6805, #6832, .T. ) ;
#7211 = CARTESIAN_POINT ( 'NONE',  ( -12.86891638962156215, 56.43380494353993271, -13.00000000000000178 ) ) ;
#7212 = ORIENTED_EDGE ( 'NONE', *, *, #6151, .F. ) ;
#7213 = CARTESIAN_POINT ( 'NONE',  ( 90.11631465359491244, 37.12029293941346708, -10.50000000000000000 ) ) ;
#7214 = CARTESIAN_POINT ( 'NONE',  ( 27.01438936481372721, 47.21331623427104063, -13.00000000000000178 ) ) ;
#7215 = AXIS2_PLACEMENT_3D ( 'NONE', #5251, #11612, #15020 ) ;
#7216 = DIRECTION ( 'NONE',  ( -1.000000000000000000, 0.000000000000000000, 0.000000000000000000 ) ) ;
#7217 = EDGE_CURVE ( 'NONE', #9394, #3039, #14328, .T. ) ;
#7218 = CARTESIAN_POINT ( 'NONE',  ( -3.333333333333330373, -2.694301256218263330, -3.300726591567081147 ) ) ;
#7219 = ADVANCED_FACE ( 'NONE', ( #6319 ), #6400, .F. ) ;
#7220 = ORIENTED_EDGE ( 'NONE', *, *, #6947, .F. ) ;
#7221 = DIRECTION ( 'NONE',  ( -0.000000000000000000, -0.000000000000000000, 1.000000000000000000 ) ) ;
#7222 = ORIENTED_EDGE ( 'NONE', *, *, #12075, .F. ) ;
#7223 = DIRECTION ( 'NONE',  ( 0.000000000000000000, 0.000000000000000000, -1.000000000000000000 ) ) ;
#7224 = DIRECTION ( 'NONE',  ( -0.000000000000000000, -0.000000000000000000, 1.000000000000000000 ) ) ;
#7225 = DIRECTION ( 'NONE',  ( -0.000000000000000000, -0.000000000000000000, -1.000000000000000000 ) ) ;
#7226 = DIRECTION ( 'NONE',  ( -0.000000000000000000, -0.000000000000000000, -1.000000000000000000 ) ) ;
#7227 = VERTEX_POINT ( 'NONE', #1641 ) ;
#7228 = CYLINDRICAL_SURFACE ( 'NONE', #2819, 59.50000000000000000 ) ;
#7229 = DIRECTION ( 'NONE',  ( 0.000000000000000000, 0.000000000000000000, 1.000000000000000000 ) ) ;
#7230 = CARTESIAN_POINT ( 'NONE',  ( -57.06275842387042729, 9.706953719246069312, -10.50000000000000000 ) ) ;
#7231 = ORIENTED_EDGE ( 'NONE', *, *, #12801, .F. ) ;
#7232 = CIRCLE ( 'NONE', #10403, 2.649999999999985700 ) ;
#7233 = ORIENTED_EDGE ( 'NONE', *, *, #7066, .T. ) ;
#7234 = DIRECTION ( 'NONE',  ( 1.000000000000000000, 0.000000000000000000, 0.000000000000000000 ) ) ;
#7235 = CARTESIAN_POINT ( 'NONE',  ( 9.115592515563379905, 106.6114291000284027, 19.74294316973679386 ) ) ;
#7236 = DIRECTION ( 'NONE',  ( 0.000000000000000000, 0.000000000000000000, -1.000000000000000000 ) ) ;
#7237 = CARTESIAN_POINT ( 'NONE',  ( -53.55662432702593634, 0.000000000000000000, -10.50000000000000000 ) ) ;
#7238 = EDGE_CURVE ( 'NONE', #331, #10950, #9704, .T. ) ;
#7239 = CARTESIAN_POINT ( 'NONE',  ( -30.18932686484984629, 96.38267619380719964, -13.21651853314490488 ) ) ;
#7240 = VERTEX_POINT ( 'NONE', #14472 ) ;
#7241 = ORIENTED_EDGE ( 'NONE', *, *, #11969, .T. ) ;
#7242 = VERTEX_POINT ( 'NONE', #4075 ) ;
#7243 = VERTEX_POINT ( 'NONE', #13321 ) ;
#7244 = LINE ( 'NONE', #10829, #5690 ) ;
#7245 = AXIS2_PLACEMENT_3D ( 'NONE', #4491, #13822, #13752 ) ;
#7246 = FACE_OUTER_BOUND ( 'NONE', #3342, .T. ) ;
#7247 = CARTESIAN_POINT ( 'NONE',  ( 12.50000000000000000, 100.2235002382176248, -15.33678752976415716 ) ) ;
#7248 = ORIENTED_EDGE ( 'NONE', *, *, #12793, .T. ) ;
#7249 = VERTEX_POINT ( 'NONE', #7544 ) ;
#7250 = DIRECTION ( 'NONE',  ( 1.000000000000000000, 0.000000000000000000, 0.000000000000000000 ) ) ;
#7251 = PRODUCT_DEFINITION_FORMATION_WITH_SPECIFIED_SOURCE ( 'ANY', '', #7917, .NOT_KNOWN. ) ;
#7252 = ORIENTED_EDGE ( 'NONE', *, *, #12933, .T. ) ;
#7253 = CIRCLE ( 'NONE', #7791, 0.5000000000000073275 ) ;
#7254 = FACE_OUTER_BOUND ( 'NONE', #13944, .T. ) ;
#7255 = EDGE_CURVE ( 'NONE', #1613, #6509, #10129, .T. ) ;
#7256 = VECTOR ( 'NONE', #14431, 1000.000000000000000 ) ;
#7257 = CARTESIAN_POINT ( 'NONE',  ( 2.725741868436124538, -3.045094352033993701, -3.220599429844053674 ) ) ;
#7258 = DIRECTION ( 'NONE',  ( 0.000000000000000000, 0.000000000000000000, 1.000000000000000000 ) ) ;
#7259 = EDGE_CURVE ( 'NONE', #331, #14939, #1576, .T. ) ;
#7260 = EDGE_CURVE ( 'NONE', #5893, #7516, #5355, .T. ) ;
#7261 = ORIENTED_EDGE ( 'NONE', *, *, #14579, .F. ) ;
#7262 = DIRECTION ( 'NONE',  ( 0.000000000000000000, 0.000000000000000000, -1.000000000000000000 ) ) ;
#7263 = CYLINDRICAL_SURFACE ( 'NONE', #13089, 10.00000000000000178 ) ;
#7264 = ORIENTED_EDGE ( 'NONE', *, *, #4500, .T. ) ;
#7265 = DIRECTION ( 'NONE',  ( 1.000000000000000000, 0.000000000000000000, 0.000000000000000000 ) ) ;
#7266 = VECTOR ( 'NONE', #12531, 1000.000000000000000 ) ;
#7267 = CIRCLE ( 'NONE', #9939, 59.50000000000000000 ) ;
#7268 = EDGE_CURVE ( 'NONE', #11211, #4485, #5573, .T. ) ;
#7269 = VERTEX_POINT ( 'NONE', #3231 ) ;
#7270 = AXIS2_PLACEMENT_3D ( 'NONE', #10033, #11035, #5262 ) ;
#7271 = COLOUR_RGB ( '', 0.09019608, 0.27058824, 0.51372549) ;
#7272 = ORIENTED_EDGE ( 'NONE', *, *, #62, .T. ) ;
#7273 = CARTESIAN_POINT ( 'NONE',  ( 3.999999999999996447, -0.7890432684750899872, -0.04868663549882019242 ) ) ;
#7274 = CYLINDRICAL_SURFACE ( 'NONE', #354, 0.5000000000000004441 ) ;
#7275 = CARTESIAN_POINT ( 'NONE',  ( 35.79340317121621240, 100.4136097276748387, -16.00000000000000355 ) ) ;
#7276 = PRESENTATION_LAYER_ASSIGNMENT (  '', '', ( #1473 ) ) ;
#7277 = AXIS2_PLACEMENT_3D ( 'NONE', #371, #13124, #5976 ) ;
#7278 = DIRECTION ( 'NONE',  ( -1.000000000000000000, 0.000000000000000000, 0.000000000000000000 ) ) ;
#7279 = CARTESIAN_POINT ( 'NONE',  ( -5.560781378645575757, 6.809993116116508640E-16, -4.000000000000000000 ) ) ;
#7280 = DIRECTION ( 'NONE',  ( 0.000000000000000000, 0.000000000000000000, -1.000000000000000000 ) ) ;
#7281 = CIRCLE ( 'NONE', #760, 60.49999999999999289 ) ;
#7282 = CARTESIAN_POINT ( 'NONE',  ( -49.57224306869049713, 6.526309611002760747, -8.000000000000000000 ) ) ;
#7283 = CONTEXT_DEPENDENT_SHAPE_REPRESENTATION ( #7746, #10101 ) ;
#7284 = AXIS2_PLACEMENT_3D ( 'NONE', #8456, #12049, #346 ) ;
#7285 = VERTEX_POINT ( 'NONE', #9982 ) ;
#7286 = FILL_AREA_STYLE_COLOUR ( '', #10440 ) ;
#7287 = ORIENTED_EDGE ( 'NONE', *, *, #3575, .T. ) ;
#7288 = ADVANCED_FACE ( 'NONE', ( #7775 ), #12417, .T. ) ;
#7289 = FACE_OUTER_BOUND ( 'NONE', #1946, .T. ) ;
#7290 = DIRECTION ( 'NONE',  ( -1.000000000000000000, 0.000000000000000000, 0.000000000000000000 ) ) ;
#7291 = AXIS2_PLACEMENT_3D ( 'NONE', #14117, #14337, #2805 ) ;
#7292 = DIRECTION ( 'NONE',  ( 1.000000000000000000, 0.000000000000000000, 0.000000000000000000 ) ) ;
#7293 = CIRCLE ( 'NONE', #2939, 2.649999999999985700 ) ;
#7294 = FACE_OUTER_BOUND ( 'NONE', #7040, .T. ) ;
#7295 = VECTOR ( 'NONE', #2528, 1000.000000000000000 ) ;
#7296 = VERTEX_POINT ( 'NONE', #14628 ) ;
#7297 = DIRECTION ( 'NONE',  ( 0.000000000000000000, 0.000000000000000000, -1.000000000000000000 ) ) ;
#7298 = ORIENTED_EDGE ( 'NONE', *, *, #6905, .T. ) ;
#7299 = CARTESIAN_POINT ( 'NONE',  ( 9.706953719245472456, 57.06275842387054098, 8.000000000000000000 ) ) ;
#7300 = CYLINDRICAL_SURFACE ( 'NONE', #10970, 2.649999999999985700 ) ;
#7301 = AXIS2_PLACEMENT_3D ( 'NONE', #1630, #12884, #12041 ) ;
#7302 = DIRECTION ( 'NONE',  ( 0.000000000000000000, 0.000000000000000000, 1.000000000000000000 ) ) ;
#7303 = DIRECTION ( 'NONE',  ( 0.000000000000000000, 0.000000000000000000, -1.000000000000000000 ) ) ;
#7304 = ADVANCED_FACE ( 'NONE', ( #11285 ), #4526, .F. ) ;
#7305 = EDGE_LOOP ( 'NONE', ( #5533, #4712, #4219, #13744, #3310 ) ) ;
#7306 = EDGE_CURVE ( 'NONE', #1809, #5203, #7847, .T. ) ;
#7307 = COLOUR_RGB ( '', 0.08235294, 0.09019608, 0.10196078) ;
#7308 = DIRECTION ( 'NONE',  ( 0.2941176470588241498, 0.9557692240748186796, 0.000000000000000000 ) ) ;
#7309 = CARTESIAN_POINT ( 'NONE',  ( 56.43380494353997534, 12.86891638962136319, -13.00000000000000178 ) ) ;
#7310 = B_SPLINE_CURVE_WITH_KNOTS ( 'NONE', 3,
 ( #12544, #4502, #2132, #13593 ),
 .UNSPECIFIED., .F., .F.,
 ( 4, 4 ),
 ( 0.000000000000000000, 0.002452478801916377609 ),
 .UNSPECIFIED. ) ;
#7311 = DIRECTION ( 'NONE',  ( -1.000000000000000000, 8.746504920891464822E-16, 0.000000000000000000 ) ) ;
#7312 = AXIS2_PLACEMENT_3D ( 'NONE', #12380, #14891, #13445 ) ;
#7313 = EDGE_LOOP ( 'NONE', ( #10166, #3037, #10289, #14124, #6795, #6313, #1360 ) ) ;
#7314 = ADVANCED_FACE ( 'NONE', ( #4227 ), #14929, .T. ) ;
#7315 = FACE_OUTER_BOUND ( 'NONE', #549, .T. ) ;
#7316 = ORIENTED_EDGE ( 'NONE', *, *, #171, .T. ) ;
#7317 = AXIS2_PLACEMENT_3D ( 'NONE', #3132, #10181, #3210 ) ;
#7318 = FACE_OUTER_BOUND ( 'NONE', #6122, .T. ) ;
#7319 = CARTESIAN_POINT ( 'NONE',  ( -52.72775723226775568, 7.383907457638128058, 10.49999999999999822 ) ) ;
#7320 = DIRECTION ( 'NONE',  ( 1.000000000000000000, 0.000000000000000000, -0.000000000000000000 ) ) ;
#7321 = DIRECTION ( 'NONE',  ( -0.000000000000000000, -0.000000000000000000, -1.000000000000000000 ) ) ;
#7322 = ORIENTED_EDGE ( 'NONE', *, *, #4882, .T. ) ;
#7323 = EDGE_LOOP ( 'NONE', ( #14696, #10759, #6129, #2994 ) ) ;
#7324 = AXIS2_PLACEMENT_3D ( 'NONE', #8454, #3769, #10738 ) ;
#7325 = EDGE_CURVE ( 'NONE', #3583, #877, #12853, .T. ) ;
#7326 = ORIENTED_EDGE ( 'NONE', *, *, #5151, .F. ) ;
#7327 = CARTESIAN_POINT ( 'NONE',  ( -22.33583958711380646, -30.74264578624812927, -25.50000000000000355 ) ) ;
#7328 = CARTESIAN_POINT ( 'NONE',  ( 51.45950017607693638, -4.121772567811421872, -13.00000000000000178 ) ) ;
#7329 = AXIS2_PLACEMENT_3D ( 'NONE', #14755, #12256, #2070 ) ;
#7330 = CARTESIAN_POINT ( 'NONE',  ( 0.000000000000000000, 0.000000000000000000, 0.000000000000000000 ) ) ;
#7331 = ORIENTED_EDGE ( 'NONE', *, *, #9057, .F. ) ;
#7332 = ORIENTED_EDGE ( 'NONE', *, *, #13781, .F. ) ;
#7333 = FACE_OUTER_BOUND ( 'NONE', #14135, .T. ) ;
#7334 = ORIENTED_EDGE ( 'NONE', *, *, #10063, .F. ) ;
#7335 = AXIS2_PLACEMENT_3D ( 'NONE', #8369, #2749, #399 ) ;
#7336 = FACE_OUTER_BOUND ( 'NONE', #245, .T. ) ;
#7337 = CIRCLE ( 'NONE', #816, 3.000000000000002665 ) ;
#7338 = DIRECTION ( 'NONE',  ( 1.000000000000000000, 0.000000000000000000, 0.000000000000000000 ) ) ;
#7339 = FACE_OUTER_BOUND ( 'NONE', #4890, .T. ) ;
#7340 = ORIENTED_EDGE ( 'NONE', *, *, #14984, .T. ) ;
#7341 = AXIS2_PLACEMENT_3D ( 'NONE', #13034, #2705, #9744 ) ;
#7342 = DIRECTION ( 'NONE',  ( 1.000000000000000000, 0.000000000000000000, 0.000000000000000000 ) ) ;
#7343 = DIRECTION ( 'NONE',  ( -0.000000000000000000, -0.000000000000000000, 1.000000000000000000 ) ) ;
#7344 = ORIENTED_EDGE ( 'NONE', *, *, #6502, .T. ) ;
#7345 = CARTESIAN_POINT ( 'NONE',  ( -32.06294366074467206, 42.50536573064442081, 10.49999999999999822 ) ) ;
#7346 = TOROIDAL_SURFACE ( 'NONE', #2500, 102.0000000000000142, 5.000000000000000000 ) ;
#7347 = ORIENTED_EDGE ( 'NONE', *, *, #6501, .T. ) ;
#7348 = VERTEX_POINT ( 'NONE', #2154 ) ;
#7349 = DIRECTION ( 'NONE',  ( -1.000000000000000000, 1.953992523340275196E-14, 0.000000000000000000 ) ) ;
#7350 = EDGE_CURVE ( 'NONE', #9753, #1331, #808, .T. ) ;
#7351 = VERTEX_POINT ( 'NONE', #5435 ) ;
#7352 = EDGE_CURVE ( 'NONE', #8099, #2594, #13098, .T. ) ;
#7353 = CIRCLE ( 'NONE', #10756, 0.5000000000000004441 ) ;
#7354 = PLANE ( 'NONE',  #494 ) ;
#7355 = CARTESIAN_POINT ( 'NONE',  ( 0.000000000000000000, 0.000000000000000000, -23.50000000000000000 ) ) ;
#7356 = CARTESIAN_POINT ( 'NONE',  ( -12.50000000000000000, 59.24038404635959409, 20.00000000000000000 ) ) ;
#7357 = DIRECTION ( 'NONE',  ( -1.000000000000000000, 0.000000000000000000, 0.000000000000000000 ) ) ;
#7358 = EDGE_CURVE ( 'NONE', #9310, #4530, #9203, .T. ) ;
#7359 = CARTESIAN_POINT ( 'NONE',  ( -0.3198814748697815791, -4.434118497892180599, -0.3507732604232504658 ) ) ;
#7360 = ORIENTED_EDGE ( 'NONE', *, *, #7072, .F. ) ;
#7361 = AXIS2_PLACEMENT_3D ( 'NONE', #3825, #6225, #1685 ) ;
#7362 = AXIS2_PLACEMENT_3D ( 'NONE', #11224, #11144, #7564 ) ;
#7363 = DIRECTION ( 'NONE',  ( 1.000000000000000000, 0.000000000000000000, 0.000000000000000000 ) ) ;
#7364 = ORIENTED_EDGE ( 'NONE', *, *, #6741, .T. ) ;
#7365 = EDGE_CURVE ( 'NONE', #27, #5421, #9448, .T. ) ;
#7366 = CYLINDRICAL_SURFACE ( 'NONE', #2579, 3.000000000000002665 ) ;
#7367 = CARTESIAN_POINT ( 'NONE',  ( -56.43380494354004639, -12.86891638962099549, -8.000000000000000000 ) ) ;
#7368 = DIRECTION ( 'NONE',  ( -1.000000000000000000, 0.000000000000000000, 0.000000000000000000 ) ) ;
#7369 = EDGE_CURVE ( 'NONE', #14085, #1445, #3645, .T. ) ;
#7370 = CARTESIAN_POINT ( 'NONE',  ( 33.49014761921571903, 11.74264578624841171, -25.50000000000000355 ) ) ;
#7371 = EDGE_LOOP ( 'NONE', ( #3712, #4928, #13196, #1377, #9432, #14846, #4399, #4724, #13588 ) ) ;
#7372 = VECTOR ( 'NONE', #360, 1000.000000000000000 ) ;
#7373 = AXIS2_PLACEMENT_3D ( 'NONE', #4695, #2478, #980 ) ;
#7374 = VECTOR ( 'NONE', #2911, 1000.000000000000000 ) ;
#7375 = CARTESIAN_POINT ( 'NONE',  ( 6.451868917687939131, 52.36539807335604024, -10.50000000000000000 ) ) ;
#7376 = AXIS2_PLACEMENT_3D ( 'NONE', #12212, #7645, #14722 ) ;
#7377 = ORIENTED_EDGE ( 'NONE', *, *, #3615, .T. ) ;
#7378 = LINE ( 'NONE', #10953, #6055 ) ;
#7379 = FACE_OUTER_BOUND ( 'NONE', #11819, .T. ) ;
#7380 = CARTESIAN_POINT ( 'NONE',  ( -33.83495342806088502, 101.3902949203996116, -15.35262818605210988 ) ) ;
#7381 = DIRECTION ( 'NONE',  ( 0.000000000000000000, -1.000000000000000000, 1.287488025362403787E-15 ) ) ;
#7382 = CARTESIAN_POINT ( 'NONE',  ( -9.449524216731115089, 94.52924706620449058, 19.61300924954587188 ) ) ;
#7383 = CIRCLE ( 'NONE', #8356, 59.50000000000000711 ) ;
#7384 = EDGE_LOOP ( 'NONE', ( #10482, #11929, #3857, #12570, #2846, #6944 ) ) ;
#7385 = VECTOR ( 'NONE', #6030, 999.9999999999998863 ) ;
#7386 = AXIS2_PLACEMENT_3D ( 'NONE', #11884, #3836, #10816 ) ;
#7387 = DIRECTION ( 'NONE',  ( 0.000000000000000000, 0.000000000000000000, 1.000000000000000000 ) ) ;
#7388 = FACE_OUTER_BOUND ( 'NONE', #6241, .T. ) ;
#7389 = CIRCLE ( 'NONE', #14681, 100.0000000000000000 ) ;
#7390 = DIRECTION ( 'NONE',  ( 0.000000000000000000, 0.000000000000000000, 1.000000000000000000 ) ) ;
#7391 = ORIENTED_EDGE ( 'NONE', *, *, #5907, .T. ) ;
#7392 = CARTESIAN_POINT ( 'NONE',  ( -31.47058823529412663, 102.2673069760056563, -79.80561291909842225 ) ) ;
#7393 = EDGE_CURVE ( 'NONE', #13229, #8152, #768, .T. ) ;
#7394 = AXIS2_PLACEMENT_3D ( 'NONE', #6078, #1316, #7368 ) ;
#7395 = ORIENTED_EDGE ( 'NONE', *, *, #2224, .F. ) ;
#7396 = EDGE_CURVE ( 'NONE', #14, #8885, #11888, .T. ) ;
#7397 = CYLINDRICAL_SURFACE ( 'NONE', #6404, 0.5000000000000004441 ) ;
#7398 = ORIENTED_EDGE ( 'NONE', *, *, #4047, .F. ) ;
#7399 = AXIS2_PLACEMENT_3D ( 'NONE', #12599, #2194, #1072 ) ;
#7400 = ADVANCED_FACE ( 'NONE', ( #253 ), #105, .F. ) ;
#7401 = CARTESIAN_POINT ( 'NONE',  ( 0.000000000000000000, 0.000000000000000000, -8.000000000000000000 ) ) ;
#7402 = CARTESIAN_POINT ( 'NONE',  ( 3.333333333333338810, -2.694301256218270435, -3.300726591567082480 ) ) ;
#7403 = DIRECTION ( 'NONE',  ( 1.000000000000000000, 0.000000000000000000, 0.000000000000000000 ) ) ;
#7404 = CARTESIAN_POINT ( 'NONE',  ( -32.35455048062396344, 95.67796756487054211, -15.49337032400452507 ) ) ;
#7405 = VERTEX_POINT ( 'NONE', #1178 ) ;
#7406 = ORIENTED_EDGE ( 'NONE', *, *, #7260, .F. ) ;
#7407 = AXIS2_PLACEMENT_3D ( 'NONE', #49, #5744, #8021 ) ;
#7408 = EDGE_CURVE ( 'NONE', #13116, #11806, #4896, .T. ) ;
#7409 = DIRECTION ( 'NONE',  ( 1.000000000000000000, 0.000000000000000000, 0.000000000000000000 ) ) ;
#7410 = FACE_OUTER_BOUND ( 'NONE', #14605, .T. ) ;
#7411 = CIRCLE ( 'NONE', #9104, 2.500000000000000444 ) ;
#7412 = CYLINDRICAL_SURFACE ( 'NONE', #6131, 3.000000000000002665 ) ;
#7413 = VERTEX_POINT ( 'NONE', #12719 ) ;
#7414 = VERTEX_POINT ( 'NONE', #3537 ) ;
#7415 = LINE ( 'NONE', #12408, #107 ) ;
#7416 = VERTEX_POINT ( 'NONE', #8077 ) ;
#7417 = EDGE_CURVE ( 'NONE', #12179, #12421, #7253, .T. ) ;
#7418 = AXIS2_PLACEMENT_3D ( 'NONE', #3460, #8081, #9367 ) ;
#7419 = CYLINDRICAL_SURFACE ( 'NONE', #8986, 59.50000000000000000 ) ;
#7420 = PRODUCT_DEFINITION_SHAPE ( 'NONE', 'NONE',  #15033 ) ;
#7421 = CARTESIAN_POINT ( 'NONE',  ( 1.243802165048770725, -3.900692638707479620, -3.223146290109812462 ) ) ;
#7422 =( NAMED_UNIT ( * ) PLANE_ANGLE_UNIT ( ) SI_UNIT ( $, .RADIAN. ) );
#7423 = DIRECTION ( 'NONE',  ( -1.000000000000000000, 0.000000000000000000, 0.000000000000000000 ) ) ;
#7424 = CARTESIAN_POINT ( 'NONE',  ( 25.00000000000000000, 81.24038404635960831, 13.50000000000000533 ) ) ;
#7425 = ORIENTED_EDGE ( 'NONE', *, *, #4089, .T. ) ;
#7426 = CARTESIAN_POINT ( 'NONE',  ( 92.55687898036906347, 36.52608637591612961, 8.000000000000000000 ) ) ;
#7427 = VECTOR ( 'NONE', #12847, 1000.000000000000000 ) ;
#7428 = ORIENTED_EDGE ( 'NONE', *, *, #1664, .F. ) ;
#7429 = ORIENTED_EDGE ( 'NONE', *, *, #142, .T. ) ;
#7430 = DIRECTION ( 'NONE',  ( -1.000000000000000000, 0.000000000000000000, 0.000000000000000000 ) ) ;
#7431 = CARTESIAN_POINT ( 'NONE',  ( 31.63177518854776338, 102.2170822241992596, -12.29884221335728967 ) ) ;
#7432 = DIRECTION ( 'NONE',  ( 0.000000000000000000, 0.000000000000000000, -1.000000000000000000 ) ) ;
#7433 = DIRECTION ( 'NONE',  ( 0.000000000000000000, 0.000000000000000000, -1.000000000000000000 ) ) ;
#7434 = DIRECTION ( 'NONE',  ( -0.000000000000000000, -0.000000000000000000, -1.000000000000000000 ) ) ;
#7435 = DIRECTION ( 'NONE',  ( 0.000000000000000000, 0.000000000000000000, 1.000000000000000000 ) ) ;
#7436 = VERTEX_POINT ( 'NONE', #1252 ) ;
#7437 = EDGE_CURVE ( 'NONE', #9373, #11092, #10420, .T. ) ;
#7438 = LINE ( 'NONE', #12161, #1235 ) ;
#7439 = VERTEX_POINT ( 'NONE', #12640 ) ;
#7440 = CARTESIAN_POINT ( 'NONE',  ( 37.53686968382241673, 89.89283556784525331, -13.00000000000000178 ) ) ;
#7441 = CYLINDRICAL_SURFACE ( 'NONE', #3718, 2.649999999999992806 ) ;
#7442 = VERTEX_POINT ( 'NONE', #6855 ) ;
#7443 = LINE ( 'NONE', #545, #7640 ) ;
#7444 = PLANE ( 'NONE',  #9304 ) ;
#7445 = ORIENTED_EDGE ( 'NONE', *, *, #13960, .T. ) ;
#7446 = FACE_OUTER_BOUND ( 'NONE', #829, .T. ) ;
#7447 = ORIENTED_EDGE ( 'NONE', *, *, #6698, .T. ) ;
#7448 = DIRECTION ( 'NONE',  ( -0.000000000000000000, -0.000000000000000000, -1.000000000000000000 ) ) ;
#7449 = LINE ( 'NONE', #1625, #14360 ) ;
#7450 = DIRECTION ( 'NONE',  ( -1.000000000000000000, 0.000000000000000000, 0.000000000000000000 ) ) ;
#7451 = CARTESIAN_POINT ( 'NONE',  ( -26.49999999999971578, -45.89934640057541060, -8.000000000000000000 ) ) ;
#7452 = EDGE_CURVE ( 'NONE', #1677, #10590, #12368, .T. ) ;
#7453 = ADVANCED_FACE ( 'NONE', ( #1112 ), #986, .F. ) ;
#7454 = CARTESIAN_POINT ( 'NONE',  ( 68.58935777509475429, -68.58935777509547904, -10.50000000000000000 ) ) ;
#7455 = AXIS2_PLACEMENT_3D ( 'NONE', #8406, #4622, #53 ) ;
#7456 = ORIENTED_EDGE ( 'NONE', *, *, #3895, .T. ) ;
#7457 = PLANE ( 'NONE',  #10586 ) ;
#7458 = DIRECTION ( 'NONE',  ( 0.000000000000000000, 0.000000000000000000, -1.000000000000000000 ) ) ;
#7459 = DIRECTION ( 'NONE',  ( -1.000000000000000000, 0.000000000000000000, 0.000000000000000000 ) ) ;
#7460 = VERTEX_POINT ( 'NONE', #181 ) ;
#7461 = B_SPLINE_CURVE_WITH_KNOTS ( 'NONE', 3,
 ( #5732, #2320, #2160, #6999, #2097, #1042, #5793, #13869, #6710, #9217 ),
 .UNSPECIFIED., .F., .F.,
 ( 4, 2, 2, 2, 4 ),
 ( 0.000000000000000000, 0.001715760189696190381, 0.003431520379392380762, 0.005147280569088571144, 0.006863040758784761525 ),
 .UNSPECIFIED. ) ;
#7462 = CARTESIAN_POINT ( 'NONE',  ( 3.999999999999996447, 2.309401076758498039, -5.000000000000000888 ) ) ;
#7463 = ORIENTED_EDGE ( 'NONE', *, *, #10741, .F. ) ;
#7464 = CARTESIAN_POINT ( 'NONE',  ( -32.46576781417928714, 41.59008834022678514, -13.00000000000000178 ) ) ;
#7465 = CARTESIAN_POINT ( 'NONE',  ( -33.48561063518626923, 47.21331623427104063, -10.50000000000000000 ) ) ;
#7466 = DIRECTION ( 'NONE',  ( -1.000000000000000000, 8.705157806719979026E-14, 0.000000000000000000 ) ) ;
#7467 = CARTESIAN_POINT ( 'NONE',  ( 55.00000000000000000, -6.735557395310442615E-15, -13.00000000000000178 ) ) ;
#7468 = APPLICATION_PROTOCOL_DEFINITION ( 'draft international standard', 'automotive_design', 1998, #3784 ) ;
#7469 = FACE_OUTER_BOUND ( 'NONE', #5817, .T. ) ;
#7470 = ORIENTED_EDGE ( 'NONE', *, *, #3100, .F. ) ;
#7471 = ORIENTED_EDGE ( 'NONE', *, *, #7202, .T. ) ;
#7472 = CARTESIAN_POINT ( 'NONE',  ( -3.941339353050220809E-13, 4.796734841935198723, -3.721909803043260467 ) ) ;
#7473 = LINE ( 'NONE', #6117, #7372 ) ;
#7474 = EDGE_CURVE ( 'NONE', #5656, #12871, #14010, .T. ) ;
#7475 = DIRECTION ( 'NONE',  ( -1.000000000000000000, 0.000000000000000000, 0.000000000000000000 ) ) ;
#7476 = ORIENTED_EDGE ( 'NONE', *, *, #12618, .F. ) ;
#7477 = EDGE_CURVE ( 'NONE', #8423, #2406, #2661, .T. ) ;
#7478 = ORIENTED_EDGE ( 'NONE', *, *, #14359, .T. ) ;
#7479 = DIRECTION ( 'NONE',  ( -0.000000000000000000, -0.000000000000000000, 1.000000000000000000 ) ) ;
#7480 = EDGE_LOOP ( 'NONE', ( #168, #7792, #2190, #873 ) ) ;
#7481 = DIRECTION ( 'NONE',  ( 1.000000000000000000, 0.000000000000000000, 0.000000000000000000 ) ) ;
#7482 = ADVANCED_FACE ( 'NONE', ( #1328 ), #7074, .T. ) ;
#7483 = CARTESIAN_POINT ( 'NONE',  ( -4.211140560182194292, -2.431303136016555122, -3.745885042887437510 ) ) ;
#7484 = CARTESIAN_POINT ( 'NONE',  ( 45.89934640057532533, -26.49999999999987566, -13.00000000000000178 ) ) ;
#7485 = CARTESIAN_POINT ( 'NONE',  ( 12.50000000000000000, 40.62019202317980415, -16.00000000000000000 ) ) ;
#7486 = ORIENTED_EDGE ( 'NONE', *, *, #10994, .F. ) ;
#7487 = CARTESIAN_POINT ( 'NONE',  ( -97.00000000000000000, 1.015776140243522349E-12, -10.50000000000000000 ) ) ;
#7488 = EDGE_CURVE ( 'NONE', #13059, #9534, #3456, .T. ) ;
#7489 = EDGE_CURVE ( 'NONE', #5951, #14678, #12404, .T. ) ;
#7490 = ORIENTED_EDGE ( 'NONE', *, *, #9493, .F. ) ;
#7491 = ORIENTED_EDGE ( 'NONE', *, *, #9672, .F. ) ;
#7492 = CARTESIAN_POINT ( 'NONE',  ( 53.26842454702428142, 11.55014193876197126, 8.000000000000000000 ) ) ;
#7493 = VECTOR ( 'NONE', #11701, 1000.000000000000000 ) ;
#7494 = VECTOR ( 'NONE', #2590, 1000.000000000000000 ) ;
#7495 = CARTESIAN_POINT ( 'NONE',  ( -37.12029293941441210, -89.61631465359452875, -8.000000000000000000 ) ) ;
#7496 = ADVANCED_FACE ( 'NONE', ( #3681 ), #8302, .F. ) ;
#7497 = CARTESIAN_POINT ( 'NONE',  ( 0.000000000000000000, 0.000000000000000000, -10.50000000000000000 ) ) ;
#7498 = DIRECTION ( 'NONE',  ( -0.000000000000000000, -0.000000000000000000, -1.000000000000000000 ) ) ;
#7499 = DIRECTION ( 'NONE',  ( -1.000000000000000000, 0.000000000000000000, 0.000000000000000000 ) ) ;
#7500 = AXIS2_PLACEMENT_3D ( 'NONE', #13239, #5035, #2834 ) ;
#7501 = DIRECTION ( 'NONE',  ( 0.000000000000000000, 0.000000000000000000, 1.000000000000000000 ) ) ;
#7502 = VERTEX_POINT ( 'NONE', #11809 ) ;
#7503 = AXIS2_PLACEMENT_3D ( 'NONE', #13710, #6476, #12568 ) ;
#7504 = AXIS2_PLACEMENT_3D ( 'NONE', #3209, #3067, #6685 ) ;
#7505 =( LENGTH_UNIT ( ) NAMED_UNIT ( * ) SI_UNIT ( .MILLI., .METRE. ) );
#7506 = DIRECTION ( 'NONE',  ( 0.000000000000000000, 0.000000000000000000, 1.000000000000000000 ) ) ;
#7507 = FACE_OUTER_BOUND ( 'NONE', #12063, .T. ) ;
#7508 = DIRECTION ( 'NONE',  ( 1.000000000000000000, 0.000000000000000000, 0.000000000000000000 ) ) ;
#7509 = EDGE_LOOP ( 'NONE', ( #3849, #10163, #8158, #4240, #8349 ) ) ;
#7510 = CARTESIAN_POINT ( 'NONE',  ( 30.33882973767905966, 96.33581297378609065, -13.50942224097978261 ) ) ;
#7511 = CIRCLE ( 'NONE', #9458, 3.000000000000002665 ) ;
#7512 = DIRECTION ( 'NONE',  ( 1.000000000000000000, 0.000000000000000000, 0.000000000000000000 ) ) ;
#7513 = VERTEX_POINT ( 'NONE', #1471 ) ;
#7514 = CARTESIAN_POINT ( 'NONE',  ( 39.30189486418243661, 33.47282819776626894, -13.00000000000000178 ) ) ;
#7515 = AXIS2_PLACEMENT_3D ( 'NONE', #2815, #7433, #1673 ) ;
#7516 = VERTEX_POINT ( 'NONE', #8668 ) ;
#7517 = AXIS2_PLACEMENT_3D ( 'NONE', #10024, #4197, #929 ) ;
#7518 = CARTESIAN_POINT ( 'NONE',  ( 0.000000000000000000, 0.000000000000000000, 13.00000000000000178 ) ) ;
#7519 = FACE_OUTER_BOUND ( 'NONE', #4114, .T. ) ;
#7520 = DIRECTION ( 'NONE',  ( 0.000000000000000000, 0.000000000000000000, 1.000000000000000000 ) ) ;
#7521 = DIRECTION ( 'NONE',  ( 0.000000000000000000, 0.000000000000000000, -1.000000000000000000 ) ) ;
#7522 = DIRECTION ( 'NONE',  ( -1.000000000000000000, 0.000000000000000000, 0.000000000000000000 ) ) ;
#7523 = VECTOR ( 'NONE', #8192, 1000.000000000000000 ) ;
#7524 = DIRECTION ( 'NONE',  ( 1.000000000000000000, 0.000000000000000000, 0.000000000000000000 ) ) ;
#7525 = CIRCLE ( 'NONE', #510, 0.5000000000000022204 ) ;
#7526 = ORIENTED_EDGE ( 'NONE', *, *, #6547, .T. ) ;
#7527 = CARTESIAN_POINT ( 'NONE',  ( 24.98583958711424202, -30.74264578624780597, -28.00000000000000000 ) ) ;
#7528 = VECTOR ( 'NONE', #2623, 999.9999999999998863 ) ;
#7529 = CARTESIAN_POINT ( 'NONE',  ( 0.000000000000000000, 0.000000000000000000, 10.50000000000000000 ) ) ;
#7530 = VECTOR ( 'NONE', #11922, 1000.000000000000000 ) ;
#7531 = DIRECTION ( 'NONE',  ( -0.000000000000000000, -0.000000000000000000, -1.000000000000000000 ) ) ;
#7532 = EDGE_CURVE ( 'NONE', #5235, #1639, #3162, .T. ) ;
#7533 = PRODUCT_DEFINITION_SHAPE ( 'NONE', 'NONE',  #3850 ) ;
#7534 = EDGE_CURVE ( 'NONE', #3488, #1441, #2420, .T. ) ;
#7535 = VERTEX_POINT ( 'NONE', #10730 ) ;
#7536 = EDGE_CURVE ( 'NONE', #11040, #11081, #3906, .T. ) ;
#7537 = EDGE_CURVE ( 'NONE', #2474, #14819, #7012, .T. ) ;
#7538 = DIRECTION ( 'NONE',  ( 0.000000000000000000, 0.000000000000000000, -1.000000000000000000 ) ) ;
#7539 = ORIENTED_EDGE ( 'NONE', *, *, #8699, .T. ) ;
#7540 = CIRCLE ( 'NONE', #30, 3.000000000000002665 ) ;
#7541 = CARTESIAN_POINT ( 'NONE',  ( 39.61975340586557337, 91.27544013909754028, -13.00000000000000178 ) ) ;
#7542 = FACE_OUTER_BOUND ( 'NONE', #14700, .T. ) ;
#7543 = ORIENTED_EDGE ( 'NONE', *, *, #10150, .F. ) ;
#7544 = CARTESIAN_POINT ( 'NONE',  ( 35.00000000000000000, 81.24038404635960831, 23.50000000000000355 ) ) ;
#7545 = AXIS2_PLACEMENT_3D ( 'NONE', #14994, #9502, #4585 ) ;
#7546 = CYLINDRICAL_SURFACE ( 'NONE', #828, 63.00000000000000000 ) ;
#7547 = ORIENTED_EDGE ( 'NONE', *, *, #9820, .T. ) ;
#7548 = EDGE_CURVE ( 'NONE', #14306, #13178, #484, .T. ) ;
#7549 = ORIENTED_EDGE ( 'NONE', *, *, #12075, .T. ) ;
#7550 =( REPRESENTATION_RELATIONSHIP ('NONE','NONE', #12187, #8006 ) REPRESENTATION_RELATIONSHIP_WITH_TRANSFORMATION ( #4797 )SHAPE_REPRESENTATION_RELATIONSHIP( ) );
#7551 = DIRECTION ( 'NONE',  ( 0.000000000000000000, 0.000000000000000000, 1.000000000000000000 ) ) ;
#7552 = CARTESIAN_POINT ( 'NONE',  ( -4.197393957002300446, -7.680494662014190109E-14, -3.503767560748928922 ) ) ;
#7553 = AXIS2_PLACEMENT_3D ( 'NONE', #13995, #2366, #12780 ) ;
#7554 = EDGE_CURVE ( 'NONE', #13671, #9453, #5579, .T. ) ;
#7555 = PLANE ( 'NONE',  #10991 ) ;
#7556 = EDGE_LOOP ( 'NONE', ( #11587, #10867, #12655, #2183 ) ) ;
#7557 = CIRCLE ( 'NONE', #1036, 100.0000000000000000 ) ;
#7558 = ORIENTED_EDGE ( 'NONE', *, *, #4433, .T. ) ;
#7559 = B_SPLINE_CURVE_WITH_KNOTS ( 'NONE', 3,
 ( #1909, #5413, #3131, #8962, #10112, #14754, #13602, #13991 ),
 .UNSPECIFIED., .F., .F.,
 ( 4, 2, 2, 4 ),
 ( 0.000000000000000000, 0.002450665683189819696, 0.003675998524784731061, 0.004901331366379641993 ),
 .UNSPECIFIED. ) ;
#7560 = EDGE_CURVE ( 'NONE', #7767, #8421, #9243, .T. ) ;
#7561 = ORIENTED_EDGE ( 'NONE', *, *, #3289, .F. ) ;
#7562 = CARTESIAN_POINT ( 'NONE',  ( -22.33583958711380646, -30.74264578624812927, -25.50000000000000355 ) ) ;
#7563 = CIRCLE ( 'NONE', #1275, 100.0000000000000000 ) ;
#7564 = DIRECTION ( 'NONE',  ( 1.000000000000000000, 0.000000000000000000, -0.000000000000000000 ) ) ;
#7565 =( NAMED_UNIT ( * ) SI_UNIT ( $, .STERADIAN. ) SOLID_ANGLE_UNIT ( ) );
#7566 = ORIENTED_EDGE ( 'NONE', *, *, #9353, .T. ) ;
#7567 = CARTESIAN_POINT ( 'NONE',  ( -7.500000000000000888, 59.24038404635959409, 15.00000000000000000 ) ) ;
#7568 = DIRECTION ( 'NONE',  ( 1.000000000000000000, 0.000000000000000000, 0.000000000000000000 ) ) ;
#7569 = AXIS2_PLACEMENT_3D ( 'NONE', #9723, #251, #2837 ) ;
#7570 = VERTEX_POINT ( 'NONE', #10809 ) ;
#7571 = CARTESIAN_POINT ( 'NONE',  ( 2.687328764639642653, -3.067272167851296860, -0.05923475698271275791 ) ) ;
#7572 = ORIENTED_EDGE ( 'NONE', *, *, #14960, .T. ) ;
#7573 = CIRCLE ( 'NONE', #2742, 59.50000000000000000 ) ;
#7574 = EDGE_LOOP ( 'NONE', ( #7463, #12648, #3870, #8109, #12248 ) ) ;
#7575 = CARTESIAN_POINT ( 'NONE',  ( 0.000000000000000000, 0.000000000000000000, -20.00000000000000000 ) ) ;
#7576 = AXIS2_PLACEMENT_3D ( 'NONE', #1682, #4044, #3746 ) ;
#7577 = LINE ( 'NONE', #5392, #7266 ) ;
#7578 = EDGE_CURVE ( 'NONE', #6497, #13693, #2702, .T. ) ;
#7579 = AXIS2_PLACEMENT_3D ( 'NONE', #14643, #5452, #13344 ) ;
#7580 = EDGE_CURVE ( 'NONE', #3803, #11690, #13134, .T. ) ;
#7581 = DIRECTION ( 'NONE',  ( 1.000000000000000000, 0.000000000000000000, -0.000000000000000000 ) ) ;
#7582 = DIRECTION ( 'NONE',  ( 0.000000000000000000, 0.000000000000000000, 1.000000000000000000 ) ) ;
#7583 = DIRECTION ( 'NONE',  ( 0.000000000000000000, 0.000000000000000000, 1.000000000000000000 ) ) ;
#7584 = CARTESIAN_POINT ( 'NONE',  ( 55.00000000000000711, 2.789133085058097101E-16, -2.055000000000000160 ) ) ;
#7585 = EDGE_CURVE ( 'NONE', #3464, #5876, #8512, .T. ) ;
#7586 = AXIS2_PLACEMENT_3D ( 'NONE', #12382, #9384, #1977 ) ;
#7587 = ORIENTED_EDGE ( 'NONE', *, *, #1380, .F. ) ;
#7588 = DIRECTION ( 'NONE',  ( 0.000000000000000000, 0.000000000000000000, -1.000000000000000000 ) ) ;
#7589 = FACE_OUTER_BOUND ( 'NONE', #7175, .T. ) ;
#7590 = EDGE_CURVE ( 'NONE', #11955, #14956, #3596, .T. ) ;
#7591 = FACE_OUTER_BOUND ( 'NONE', #2648, .T. ) ;
#7592 = DIRECTION ( 'NONE',  ( 0.000000000000000000, 0.000000000000000000, 1.000000000000000000 ) ) ;
#7593 = CIRCLE ( 'NONE', #3968, 52.50000000000000711 ) ;
#7594 = ORIENTED_EDGE ( 'NONE', *, *, #11866, .T. ) ;
#7595 = CARTESIAN_POINT ( 'NONE',  ( 29.70588235294118462, 96.53269163155671606, -11.33021639467929731 ) ) ;
#7596 = ORIENTED_EDGE ( 'NONE', *, *, #11684, .T. ) ;
#7597 = DIRECTION ( 'NONE',  ( -0.000000000000000000, -0.000000000000000000, 1.000000000000000000 ) ) ;
#7598 = ORIENTED_EDGE ( 'NONE', *, *, #13487, .T. ) ;
#7599 = CARTESIAN_POINT ( 'NONE',  ( -2.100000000000000089, 2.571758278209443929E-16, -4.694516984716113228 ) ) ;
#7600 = ORIENTED_EDGE ( 'NONE', *, *, #6262, .T. ) ;
#7601 = EDGE_CURVE ( 'NONE', #11178, #6334, #2914, .T. ) ;
#7602 = VECTOR ( 'NONE', #12927, 1000.000000000000000 ) ;
#7603 = DIRECTION ( 'NONE',  ( 0.000000000000000000, 0.000000000000000000, 1.000000000000000000 ) ) ;
#7604 = PLANE ( 'NONE',  #6788 ) ;
#7605 = CARTESIAN_POINT ( 'NONE',  ( -97.00000000000000000, 1.015776140243522349E-12, 8.000000000000000000 ) ) ;
#7606 = AXIS2_PLACEMENT_3D ( 'NONE', #8585, #11801, #13010 ) ;
#7607 = CIRCLE ( 'NONE', #10766, 59.50000000000000000 ) ;
#7608 = DIRECTION ( 'NONE',  ( -1.000000000000000000, 0.000000000000000000, 0.000000000000000000 ) ) ;
#7609 = CARTESIAN_POINT ( 'NONE',  ( 49.11971303961677648, 15.88467684210564990, -8.000000000000000000 ) ) ;
#7610 = CARTESIAN_POINT ( 'NONE',  ( -10.88232432232081770, 94.37491168429329491, 18.69329470938989957 ) ) ;
#7611 = VERTEX_POINT ( 'NONE', #13090 ) ;
#7612 = CARTESIAN_POINT ( 'NONE',  ( 89.61631465359491244, 37.12029293941346708, 10.49999999999999822 ) ) ;
#7613 = DIRECTION ( 'NONE',  ( 0.000000000000000000, 0.000000000000000000, -1.000000000000000000 ) ) ;
#7614 = AXIS2_PLACEMENT_3D ( 'NONE', #8622, #1647, #1799 ) ;
#7615 = CARTESIAN_POINT ( 'NONE',  ( 3.999999999999998224, 1.658577278524641763, -3.531553309554042119 ) ) ;
#7616 = CIRCLE ( 'NONE', #14908, 60.50000000000000000 ) ;
#7617 = CONICAL_SURFACE ( 'NONE', #4004, 4.000000000000000000, 0.8911886515913786111 ) ;
#7618 = ORIENTED_EDGE ( 'NONE', *, *, #13919, .F. ) ;
#7619 = DIRECTION ( 'NONE',  ( -0.000000000000000000, -0.000000000000000000, -1.000000000000000000 ) ) ;
#7620 = ORIENTED_EDGE ( 'NONE', *, *, #12764, .T. ) ;
#7621 = CARTESIAN_POINT ( 'NONE',  ( 0.000000000000000000, 0.000000000000000000, -8.000000000000000000 ) ) ;
#7622 = FACE_OUTER_BOUND ( 'NONE', #6607, .T. ) ;
#7623 = VERTEX_POINT ( 'NONE', #10873 ) ;
#7624 = AXIS2_PLACEMENT_3D ( 'NONE', #10195, #7479, #14842 ) ;
#7625 = FACE_OUTER_BOUND ( 'NONE', #8174, .T. ) ;
#7626 = DIRECTION ( 'NONE',  ( -1.000000000000000000, 0.000000000000000000, 0.000000000000000000 ) ) ;
#7627 = SHAPE_DEFINITION_REPRESENTATION ( #14841, #12187 ) ;
#7628 = ORIENTED_EDGE ( 'NONE', *, *, #10648, .T. ) ;
#7629 = AXIS2_PLACEMENT_3D ( 'NONE', #7327, #4834, #14398 ) ;
#7630 = EDGE_CURVE ( 'NONE', #5584, #11834, #6053, .T. ) ;
#7631 = AXIS2_PLACEMENT_3D ( 'NONE', #12395, #14684, #4508 ) ;
#7632 = ORIENTED_EDGE ( 'NONE', *, *, #7255, .F. ) ;
#7633 = ORIENTED_EDGE ( 'NONE', *, *, #8552, .T. ) ;
#7634 = EDGE_CURVE ( 'NONE', #11672, #1517, #1550, .T. ) ;
#7635 = FACE_OUTER_BOUND ( 'NONE', #9224, .T. ) ;
#7637 = EDGE_CURVE ( 'NONE', #1115, #11359, #2679, .T. ) ;
#7636 = CARTESIAN_POINT ( 'NONE',  ( 31.71893208106492423, 102.1896529572239558, 12.62523369519216665 ) ) ;
#7638 = CARTESIAN_POINT ( 'NONE',  ( 25.00000000000000000, 81.24038404635960831, 23.50000000000000355 ) ) ;
#7639 = ORIENTED_EDGE ( 'NONE', *, *, #4180, .F. ) ;
#7640 = VECTOR ( 'NONE', #12092, 1000.000000000000000 ) ;
#7641 = ORIENTED_EDGE ( 'NONE', *, *, #7369, .T. ) ;
#7642 = AXIS2_PLACEMENT_3D ( 'NONE', #7309, #11966, #481 ) ;
#7643 = AXIS2_PLACEMENT_3D ( 'NONE', #5610, #2122, #8800 ) ;
#7644 = ORIENTED_EDGE ( 'NONE', *, *, #10927, .F. ) ;
#7645 = DIRECTION ( 'NONE',  ( -0.000000000000000000, -0.000000000000000000, 1.000000000000000000 ) ) ;
#7646 = DIRECTION ( 'NONE',  ( -0.000000000000000000, -0.000000000000000000, -1.000000000000000000 ) ) ;
#7647 = APPLICATION_CONTEXT ( 'automotive_design' ) ;
#7648 = EDGE_CURVE ( 'NONE', #1076, #9534, #7267, .T. ) ;
#7649 = LINE ( 'NONE', #3249, #14966 ) ;
#7650 = AXIS2_PLACEMENT_3D ( 'NONE', #6322, #13410, #9833 ) ;
#7651 = TOROIDAL_SURFACE ( 'NONE', #11556, 17.00000000000001066, 5.000000000000000000 ) ;
#7652 = FACE_BOUND ( 'NONE', #12935, .T. ) ;
#7653 = FACE_OUTER_BOUND ( 'NONE', #13806, .T. ) ;
#7654 = ORIENTED_EDGE ( 'NONE', *, *, #9057, .T. ) ;
#7655 = ADVANCED_FACE ( 'NONE', ( #1911 ), #12551, .T. ) ;
#7656 = EDGE_CURVE ( 'NONE', #12197, #8810, #14563, .T. ) ;
#7657 = CARTESIAN_POINT ( 'NONE',  ( -65.64523757230321621, -68.01302780753330524, -13.00000000000000178 ) ) ;
#7658 = ORIENTED_EDGE ( 'NONE', *, *, #3011, .F. ) ;
#7659 = ORIENTED_EDGE ( 'NONE', *, *, #14359, .F. ) ;
#7660 = CARTESIAN_POINT ( 'NONE',  ( -29.86020745210522875, 96.48508785265609333, 12.30285360678859696 ) ) ;
#7661 = AXIS2_PLACEMENT_3D ( 'NONE', #8452, #3610, #11965 ) ;
#7662 = DIRECTION ( 'NONE',  ( 0.000000000000000000, 0.000000000000000000, -1.000000000000000000 ) ) ;
#7663 = CARTESIAN_POINT ( 'NONE',  ( 0.000000000000000000, 0.000000000000000000, -8.000000000000000000 ) ) ;
#7664 = CARTESIAN_POINT ( 'NONE',  ( 2.500000000000002220, -6.938893903907228378E-15, -2.042000000000002036 ) ) ;
#7665 = PLANE ( 'NONE',  #14527 ) ;
#7666 = ORIENTED_EDGE ( 'NONE', *, *, #13061, .T. ) ;
#7667 = AXIS2_PLACEMENT_3D ( 'NONE', #5563, #3521, #4516 ) ;
#7668 = CARTESIAN_POINT ( 'NONE',  ( 0.000000000000000000, 0.000000000000000000, -10.50000000000000000 ) ) ;
#7669 = DIRECTION ( 'NONE',  ( -0.000000000000000000, -0.000000000000000000, -1.000000000000000000 ) ) ;
#7670 = EDGE_CURVE ( 'NONE', #12050, #7980, #13839, .T. ) ;
#7671 = CARTESIAN_POINT ( 'NONE',  ( 0.6937372685066667266, -4.453844082567734119, -3.610536846335893113 ) ) ;
#7672 = EDGE_CURVE ( 'NONE', #7167, #13653, #13340, .T. ) ;
#7673 = ADVANCED_FACE ( 'NONE', ( #14524 ), #788, .F. ) ;
#7674 = ORIENTED_EDGE ( 'NONE', *, *, #4218, .F. ) ;
#7675 = CARTESIAN_POINT ( 'NONE',  ( 0.000000000000000000, 5.051668046482832750E-16, -4.000000000000000000 ) ) ;
#7676 = ADVANCED_FACE ( 'NONE', ( #4125 ), #4289, .T. ) ;
#7677 = ORIENTED_EDGE ( 'NONE', *, *, #1188, .T. ) ;
#7678 = VECTOR ( 'NONE', #1614, 1000.000000000000000 ) ;
#7679 = CARTESIAN_POINT ( 'NONE',  ( 68.58935777509523746, 68.58935777509499587, -13.00000000000000178 ) ) ;
#7680 = EDGE_LOOP ( 'NONE', ( #75, #9677, #9135 ) ) ;
#7681 = ORIENTED_EDGE ( 'NONE', *, *, #8905, .F. ) ;
#7682 = DIRECTION ( 'NONE',  ( 0.000000000000000000, 0.000000000000000000, 1.000000000000000000 ) ) ;
#7683 = CARTESIAN_POINT ( 'NONE',  ( 2.500000000000002220, 1.768423874527823347, 1.020999999999994134 ) ) ;
#7684 = CARTESIAN_POINT ( 'NONE',  ( 52.72775723226780542, -7.383907457637739036, -13.00000000000000178 ) ) ;
#7685 = ADVANCED_FACE ( 'NONE', ( #13530 ), #13384, .F. ) ;
#7686 = DIRECTION ( 'NONE',  ( -0.000000000000000000, -0.000000000000000000, -1.000000000000000000 ) ) ;
#7687 = DIRECTION ( 'NONE',  ( -1.000000000000000000, 0.000000000000000000, 0.000000000000000000 ) ) ;
#7688 = VERTEX_POINT ( 'NONE', #5334 ) ;
#7689 = PLANE ( 'NONE',  #6199 ) ;
#7690 = DIRECTION ( 'NONE',  ( -0.000000000000000000, 0.000000000000000000, 1.000000000000000000 ) ) ;
#7691 = ADVANCED_FACE ( 'NONE', ( #3134 ), #10184, .T. ) ;
#7692 = EDGE_CURVE ( 'NONE', #9024, #8856, #12398, .T. ) ;
#7693 = DIRECTION ( 'NONE',  ( 0.000000000000000000, 0.000000000000000000, 1.000000000000000000 ) ) ;
#7694 = ORIENTED_EDGE ( 'NONE', *, *, #8614, .T. ) ;
#7695 = LINE ( 'NONE', #13542, #3193 ) ;
#7696 = ORIENTED_EDGE ( 'NONE', *, *, #14556, .T. ) ;
#7697 = FACE_OUTER_BOUND ( 'NONE', #1790, .T. ) ;
#7698 =( LENGTH_UNIT ( ) NAMED_UNIT ( * ) SI_UNIT ( .MILLI., .METRE. ) );
#7699 = B_SPLINE_CURVE_WITH_KNOTS ( 'NONE', 3,
 ( #4963, #7218, #12930, #14364, #3971 ),
 .UNSPECIFIED., .F., .F.,
 ( 4, 1, 4 ),
 ( 0.000000000000000000, 0.002309401076758505790, 0.004618802153517011580 ),
 .UNSPECIFIED. ) ;
#7700 = DIRECTION ( 'NONE',  ( -0.000000000000000000, -0.000000000000000000, 1.000000000000000000 ) ) ;
#7701 = FACE_OUTER_BOUND ( 'NONE', #2802, .T. ) ;
#7702 =( LENGTH_UNIT ( ) NAMED_UNIT ( * ) SI_UNIT ( .MILLI., .METRE. ) );
#7703 = ORIENTED_EDGE ( 'NONE', *, *, #1294, .T. ) ;
#7704 = ORIENTED_EDGE ( 'NONE', *, *, #3287, .F. ) ;
#7705 = LINE ( 'NONE', #734, #11553 ) ;
#7706 = LINE ( 'NONE', #12573, #3035 ) ;
#7707 = CARTESIAN_POINT ( 'NONE',  ( 0.000000000000000000, 0.000000000000000000, 0.000000000000000000 ) ) ;
#7708 = EDGE_LOOP ( 'NONE', ( #9912, #1041, #12748, #7174, #3018, #12625, #6008, #1644 ) ) ;
#7709 = ORIENTED_EDGE ( 'NONE', *, *, #7112, .T. ) ;
#7710 = EDGE_LOOP ( 'NONE', ( #4066, #10920, #5348, #8639 ) ) ;
#7711 = DIRECTION ( 'NONE',  ( 0.000000000000000000, 0.000000000000000000, 1.000000000000000000 ) ) ;
#7712 = DIRECTION ( 'NONE',  ( -0.000000000000000000, -0.000000000000000000, 1.000000000000000000 ) ) ;
#7713 =( NAMED_UNIT ( * ) SI_UNIT ( $, .STERADIAN. ) SOLID_ANGLE_UNIT ( ) );
#7714 = CARTESIAN_POINT ( 'NONE',  ( -68.01302780753309207, 65.64523757230344359, 8.000000000000000000 ) ) ;
#7715 = ORIENTED_EDGE ( 'NONE', *, *, #14715, .F. ) ;
#7716 = CARTESIAN_POINT ( 'NONE',  ( 37.12029293941315444, -89.61631465359504034, -13.00000000000000178 ) ) ;
#7717 = CARTESIAN_POINT ( 'NONE',  ( -35.79340317121619819, 100.4136097276748103, 16.00000000000000000 ) ) ;
#7718 = ORIENTED_EDGE ( 'NONE', *, *, #6232, .F. ) ;
#7719 = CARTESIAN_POINT ( 'NONE',  ( 3.999999999999996447, -2.309401076758518911, -0.5000000000000004441 ) ) ;
#7720 = VERTEX_POINT ( 'NONE', #12257 ) ;
#7721 = ORIENTED_EDGE ( 'NONE', *, *, #9655, .F. ) ;
#7722 = DIRECTION ( 'NONE',  ( 1.000000000000000000, 0.000000000000000000, 0.000000000000000000 ) ) ;
#7723 = EDGE_CURVE ( 'NONE', #11013, #5269, #13463, .T. ) ;
#7724 = EDGE_CURVE ( 'NONE', #13551, #14933, #9426, .T. ) ;
#7725 = ADVANCED_FACE ( 'NONE', ( #869 ), #5491, .T. ) ;
#7726 = LINE ( 'NONE', #12373, #10663 ) ;
#7727 = AXIS2_PLACEMENT_3D ( 'NONE', #2663, #4951, #9780 ) ;
#7728 = UNCERTAINTY_MEASURE_WITH_UNIT (LENGTH_MEASURE( 1.000000000000000082E-05 ), #7505, 'distance_accuracy_value', 'NONE');
#7729 = DIRECTION ( 'NONE',  ( -1.000000000000000000, 0.000000000000000000, 0.000000000000000000 ) ) ;
#7730 = CARTESIAN_POINT ( 'NONE',  ( 96.58511096861892042, 0.2790467552928839190, 10.49999999999999822 ) ) ;
#7731 = EDGE_CURVE ( 'NONE', #2566, #6431, #5560, .T. ) ;
#7732 = CARTESIAN_POINT ( 'NONE',  ( 55.00000000000000711, 0.000000000000000000, 0.000000000000000000 ) ) ;
#7733 = ORIENTED_EDGE ( 'NONE', *, *, #9718, .T. ) ;
#7734 = AXIS2_PLACEMENT_3D ( 'NONE', #577, #10893, #1716 ) ;
#7735 = DIRECTION ( 'NONE',  ( 0.000000000000000000, 0.000000000000000000, 1.000000000000000000 ) ) ;
#7736 = LINE ( 'NONE', #4837, #5180 ) ;
#7737 = AXIS2_PLACEMENT_3D ( 'NONE', #14265, #10916, #8266 ) ;
#7738 = CARTESIAN_POINT ( 'NONE',  ( -2.449848172108558764, -3.432307619358751172, -3.503702292528908302 ) ) ;
#7739 = EDGE_LOOP ( 'NONE', ( #10108, #1943, #13311, #8867, #1532, #2112, #2841 ) ) ;
#7740 = CARTESIAN_POINT ( 'NONE',  ( 2.100000000000000089, 0.000000000000000000, -0.2800830152838856835 ) ) ;
#7741 = ORIENTED_EDGE ( 'NONE', *, *, #12480, .T. ) ;
#7742 = DIRECTION ( 'NONE',  ( -0.8660254037844373753, 0.5000000000000021094, 0.000000000000000000 ) ) ;
#7743 = ORIENTED_EDGE ( 'NONE', *, *, #13925, .T. ) ;
#7744 = DIRECTION ( 'NONE',  ( -1.000000000000000000, 0.000000000000000000, 0.000000000000000000 ) ) ;
#7745 = AXIS2_PLACEMENT_3D ( 'NONE', #2894, #330, #1765 ) ;
#7746 =( REPRESENTATION_RELATIONSHIP ('NONE','NONE', #12187, #5964 ) REPRESENTATION_RELATIONSHIP_WITH_TRANSFORMATION ( #9487 )SHAPE_REPRESENTATION_RELATIONSHIP( ) );
#7747 = DIRECTION ( 'NONE',  ( -0.000000000000000000, -0.000000000000000000, 1.000000000000000000 ) ) ;
#7749 = CARTESIAN_POINT ( 'NONE',  ( 0.2500000000000002220, 0.000000000000000000, 0.000000000000000000 ) ) ;
#7748 = AXIS2_PLACEMENT_3D ( 'NONE', #10206, #14850, #3372 ) ;
#7750 = DIRECTION ( 'NONE',  ( 1.000000000000000000, 0.000000000000000000, 0.000000000000000000 ) ) ;
#7751 = VECTOR ( 'NONE', #12097, 1000.000000000000000 ) ;
#7752 = DIRECTION ( 'NONE',  ( 1.000000000000000000, 0.000000000000000000, 0.000000000000000000 ) ) ;
#7753 = EDGE_CURVE ( 'NONE', #11882, #2381, #3288, .T. ) ;
#7755 = DIRECTION ( 'NONE',  ( 0.000000000000000000, 0.000000000000000000, 1.000000000000000000 ) ) ;
#7754 = VECTOR ( 'NONE', #1162, 1000.000000000000000 ) ;
#7756 = EDGE_LOOP ( 'NONE', ( #14126, #8694, #14496, #2013, #2709 ) ) ;
#7757 = SURFACE_STYLE_USAGE ( .BOTH. , #12400 ) ;
#7758 = ORIENTED_EDGE ( 'NONE', *, *, #7417, .F. ) ;
#7759 = DIRECTION ( 'NONE',  ( 0.000000000000000000, 0.000000000000000000, 1.000000000000000000 ) ) ;
#7760 = CARTESIAN_POINT ( 'NONE',  ( 11.92530613726453659, 94.24865542230074311, -17.34466199971670264 ) ) ;
#7761 = AXIS2_PLACEMENT_3D ( 'NONE', #5989, #11575, #1159 ) ;
#7762 = CYLINDRICAL_SURFACE ( 'NONE', #1768, 63.00000000000000000 ) ;
#7763 = AXIS2_PLACEMENT_3D ( 'NONE', #2105, #13286, #14945 ) ;
#7764 = ORIENTED_EDGE ( 'NONE', *, *, #6657, .F. ) ;
#7765 = CARTESIAN_POINT ( 'NONE',  ( 9.706953719245472456, 57.06275842387054098, -13.00000000000000178 ) ) ;
#7766 = AXIS2_PLACEMENT_3D ( 'NONE', #4933, #4848, #2493 ) ;
#7767 = VERTEX_POINT ( 'NONE', #11414 ) ;
#7768 = DIRECTION ( 'NONE',  ( 0.000000000000000000, 0.000000000000000000, 1.000000000000000000 ) ) ;
#7769 = VERTEX_POINT ( 'NONE', #4796 ) ;
#7770 = CARTESIAN_POINT ( 'NONE',  ( 37.12029293941379393, 89.61631465359479876, 10.49999999999999822 ) ) ;
#7771 = CARTESIAN_POINT ( 'NONE',  ( 12.86891638962116247, -56.43380494354001087, -8.000000000000000000 ) ) ;
#7772 = CIRCLE ( 'NONE', #13117, 3.000000000000002665 ) ;
#7773 = EDGE_CURVE ( 'NONE', #944, #1495, #12111, .T. ) ;
#7774 = AXIS2_PLACEMENT_3D ( 'NONE', #14660, #12452, #13579 ) ;
#7775 = FACE_OUTER_BOUND ( 'NONE', #375, .T. ) ;
#7776 = ADVANCED_FACE ( 'NONE', ( #5928 ), #7055, .F. ) ;
#7777 = DIRECTION ( 'NONE',  ( 0.000000000000000000, 0.000000000000000000, 1.000000000000000000 ) ) ;
#7778 = CONTEXT_DEPENDENT_SHAPE_REPRESENTATION ( #3599, #4297 ) ;
#7779 = ORIENTED_EDGE ( 'NONE', *, *, #13043, .T. ) ;
#7780 = AXIS2_PLACEMENT_3D ( 'NONE', #7401, #10823, #3845 ) ;
#7781 = ORIENTED_EDGE ( 'NONE', *, *, #978, .F. ) ;
#7782 = EDGE_LOOP ( 'NONE', ( #3181, #10859, #8472, #2808, #1256, #9013, #10232 ) ) ;
#7783 = VECTOR ( 'NONE', #4323, 1000.000000000000000 ) ;
#7784 = CARTESIAN_POINT ( 'NONE',  ( -100.0000000000000000, 0.000000000000000000, 13.00000000000000178 ) ) ;
#7785 = CARTESIAN_POINT ( 'NONE',  ( 33.08820577230234505, 101.7009610928536887, 14.78158739605038896 ) ) ;
#7786 = DIRECTION ( 'NONE',  ( -1.000000000000000000, 0.000000000000000000, 0.000000000000000000 ) ) ;
#7787 = EDGE_LOOP ( 'NONE', ( #6257, #3937, #3765, #4402, #14995 ) ) ;
#7788 = ADVANCED_FACE ( 'NONE', ( #6915 ), #10565, .T. ) ;
#7789 = CIRCLE ( 'NONE', #1251, 3.000000000000002665 ) ;
#7790 = ORIENTED_EDGE ( 'NONE', *, *, #4764, .F. ) ;
#7791 = AXIS2_PLACEMENT_3D ( 'NONE', #2455, #8221, #6013 ) ;
#7792 = ORIENTED_EDGE ( 'NONE', *, *, #3721, .T. ) ;
#7793 = FACE_OUTER_BOUND ( 'NONE', #7680, .T. ) ;
#7794 = EDGE_CURVE ( 'NONE', #8824, #13003, #12352, .T. ) ;
#7795 = CARTESIAN_POINT ( 'NONE',  ( 37.12029293941315444, -89.61631465359504034, -8.000000000000000000 ) ) ;
#7796 = DIRECTION ( 'NONE',  ( -1.000000000000000000, 0.000000000000000000, 0.000000000000000000 ) ) ;
#7797 = ORIENTED_EDGE ( 'NONE', *, *, #15003, .T. ) ;
#7799 = PRESENTATION_LAYER_ASSIGNMENT (  '', '', ( #11202 ) ) ;
#7798 = FACE_BOUND ( 'NONE', #4292, .T. ) ;
#7800 = CARTESIAN_POINT ( 'NONE',  ( 0.000000000000000000, 0.000000000000000000, -20.00000000000000000 ) ) ;
#7801 = ORIENTED_EDGE ( 'NONE', *, *, #4865, .T. ) ;
#7802 = EDGE_LOOP ( 'NONE', ( #14444, #8583, #6027, #8749 ) ) ;
#7803 = EDGE_LOOP ( 'NONE', ( #14258, #13718, #8125, #2506 ) ) ;
#7804 = DIRECTION ( 'NONE',  ( 1.000000000000000000, 0.000000000000000000, 0.000000000000000000 ) ) ;
#7805 = DIRECTION ( 'NONE',  ( 1.000000000000000000, 0.000000000000000000, 0.000000000000000000 ) ) ;
#7806 = CARTESIAN_POINT ( 'NONE',  ( 0.000000000000000000, 0.000000000000000000, -8.000000000000000000 ) ) ;
#7807 = AXIS2_PLACEMENT_3D ( 'NONE', #8448, #1470, #2685 ) ;
#7808 = DIRECTION ( 'NONE',  ( 0.000000000000000000, 0.000000000000000000, 1.000000000000000000 ) ) ;
#7809 = CARTESIAN_POINT ( 'NONE',  ( 0.000000000000000000, 0.000000000000000000, 16.00000000000000000 ) ) ;
#7810 = CARTESIAN_POINT ( 'NONE',  ( -45.89934640057513349, 26.50000000000019540, 8.000000000000000000 ) ) ;
#7811 = VERTEX_POINT ( 'NONE', #1388 ) ;
#7812 = PLANE ( 'NONE',  #756 ) ;
#7813 = CIRCLE ( 'NONE', #5630, 3.000000000000002665 ) ;
#7814 = EDGE_CURVE ( 'NONE', #5448, #14675, #1199, .T. ) ;
#7815 = CARTESIAN_POINT ( 'NONE',  ( 0.000000000000000000, 0.000000000000000000, 20.00000000000000000 ) ) ;
#7816 = CYLINDRICAL_SURFACE ( 'NONE', #14815, 3.000000000000002665 ) ;
#7817 = ADVANCED_FACE ( 'NONE', ( #9192 ), #3589, .F. ) ;
#7818 = ORIENTED_EDGE ( 'NONE', *, *, #7023, .F. ) ;
#7819 = CARTESIAN_POINT ( 'NONE',  ( 7.500000000000000000, 94.70348462437907244, 20.00000000000000000 ) ) ;
#7820 = CIRCLE ( 'NONE', #3722, 2.649999999999989253 ) ;
#7821 = FACE_OUTER_BOUND ( 'NONE', #12009, .T. ) ;
#7822 = ORIENTED_EDGE ( 'NONE', *, *, #172, .F. ) ;
#7823 = ADVANCED_BREP_SHAPE_REPRESENTATION ( '', ( #4169, #5108 ), #6780 ) ;
#7824 = FACE_OUTER_BOUND ( 'NONE', #3856, .T. ) ;
#7825 = CIRCLE ( 'NONE', #11235, 0.5000000000000004441 ) ;
#7826 = CARTESIAN_POINT ( 'NONE',  ( -11.10542050108867329, 94.34972528831985983, -18.51161449521946523 ) ) ;
#7827 = FACE_OUTER_BOUND ( 'NONE', #6407, .T. ) ;
#7828 = CARTESIAN_POINT ( 'NONE',  ( 3.333333333333331261, 2.694301256218251339, -3.300726591567078483 ) ) ;
#7829 = DIRECTION ( 'NONE',  ( -1.000000000000000000, 0.000000000000000000, 0.000000000000000000 ) ) ;
#7830 = FACE_OUTER_BOUND ( 'NONE', #1197, .T. ) ;
#7831 = ADVANCED_FACE ( 'NONE', ( #12623 ), #5709, .T. ) ;
#7832 = FILL_AREA_STYLE ('',( #5561 ) ) ;
#7833 = ORIENTED_EDGE ( 'NONE', *, *, #3691, .T. ) ;
#7834 = ADVANCED_FACE ( 'NONE', ( #6980 ), #4110, .T. ) ;
#7835 = FACE_OUTER_BOUND ( 'NONE', #5622, .T. ) ;
#7836 = CARTESIAN_POINT ( 'NONE',  ( 9.707422895060663137, 94.50306011459642264, -19.49540453443647436 ) ) ;
#7837 = VECTOR ( 'NONE', #361, 1000.000000000000000 ) ;
#7838 = CARTESIAN_POINT ( 'NONE',  ( 49.00442420935993226, -30.80502811811213704, -10.50000000000000000 ) ) ;
#7839 = CARTESIAN_POINT ( 'NONE',  ( -27.94117647058823550, 90.79807628710781842, -16.00000000000000000 ) ) ;
#7840 = ORIENTED_EDGE ( 'NONE', *, *, #14012, .T. ) ;
#7841 = VECTOR ( 'NONE', #2148, 1000.000000000000000 ) ;
#7842 = CARTESIAN_POINT ( 'NONE',  ( -0.5449313310646759501, -4.304185902836972666, -3.316620875263518453 ) ) ;
#7843 = ORIENTED_EDGE ( 'NONE', *, *, #10812, .T. ) ;
#7844 = CARTESIAN_POINT ( 'NONE',  ( -12.50000000000000000, 59.24038404635959409, 20.00000000000000000 ) ) ;
#7845 = CARTESIAN_POINT ( 'NONE',  ( 0.000000000000000000, 0.000000000000000000, -8.000000000000000000 ) ) ;
#7846 = ORIENTED_EDGE ( 'NONE', *, *, #880, .F. ) ;
#7847 = LINE ( 'NONE', #7927, #2665 ) ;
#7848 = DIRECTION ( 'NONE',  ( -0.000000000000000000, -0.000000000000000000, -1.000000000000000000 ) ) ;
#7849 = ORIENTED_EDGE ( 'NONE', *, *, #254, .T. ) ;
#7850 = EDGE_LOOP ( 'NONE', ( #4192, #14484, #2612, #13911 ) ) ;
#7851 = AXIS2_PLACEMENT_3D ( 'NONE', #4294, #7690, #798 ) ;
#7852 = CIRCLE ( 'NONE', #11996, 4.000000000000000000 ) ;
#7853 = DIRECTION ( 'NONE',  ( -1.000000000000000000, 0.000000000000000000, 0.000000000000000000 ) ) ;
#7854 = CARTESIAN_POINT ( 'NONE',  ( 9.706953719245472456, 57.06275842387054098, 10.49999999999999822 ) ) ;
#7855 = AXIS2_PLACEMENT_3D ( 'NONE', #11537, #9299, #6717 ) ;
#7856 = DIRECTION ( 'NONE',  ( 0.000000000000000000, 0.000000000000000000, -1.000000000000000000 ) ) ;
#7857 = EDGE_LOOP ( 'NONE', ( #3408, #13954, #5438, #4607 ) ) ;
#7858 = EDGE_CURVE ( 'NONE', #5275, #6515, #4651, .T. ) ;
#7859 = ADVANCED_FACE ( 'NONE', ( #1229 ), #14724, .F. ) ;
#7860 = EDGE_LOOP ( 'NONE', ( #8541, #14477, #901, #3872, #414, #8624, #13741, #13585 ) ) ;
#7861 = CIRCLE ( 'NONE', #7127, 3.000000000000002665 ) ;
#7862 = EDGE_LOOP ( 'NONE', ( #12689, #848, #2289, #4720 ) ) ;
#7863 = AXIS2_PLACEMENT_3D ( 'NONE', #4477, #5890, #3329 ) ;
#7864 = VECTOR ( 'NONE', #9368, 1000.000000000000000 ) ;
#7865 = FACE_OUTER_BOUND ( 'NONE', #12094, .T. ) ;
#7866 = CIRCLE ( 'NONE', #1335, 95.00000000000001421 ) ;
#7867 = CARTESIAN_POINT ( 'NONE',  ( 42.04772703543530099, 32.26435573746242369, -8.000000000000000000 ) ) ;
#7868 = DIRECTION ( 'NONE',  ( 0.000000000000000000, 0.000000000000000000, 1.000000000000000000 ) ) ;
#7869 =( NAMED_UNIT ( * ) SI_UNIT ( $, .STERADIAN. ) SOLID_ANGLE_UNIT ( ) );
#7870 = DIRECTION ( 'NONE',  ( 1.000000000000000000, 0.000000000000000000, 0.000000000000000000 ) ) ;
#7871 = EDGE_CURVE ( 'NONE', #13429, #12128, #14982, .T. ) ;
#7872 = ORIENTED_EDGE ( 'NONE', *, *, #9032, .F. ) ;
#7873 = CARTESIAN_POINT ( 'NONE',  ( 46.33974596215558961, -6.205269775947987555E-15, -28.00000000000000000 ) ) ;
#7874 = CARTESIAN_POINT ( 'NONE',  ( 4.211140560182194292, -2.431303136016555122, -3.745885042887437510 ) ) ;
#7875 = ORIENTED_EDGE ( 'NONE', *, *, #11512, .F. ) ;
#7876 = VERTEX_POINT ( 'NONE', #8060 ) ;
#7877 = CARTESIAN_POINT ( 'NONE',  ( 0.000000000000000000, 0.000000000000000000, -8.000000000000000000 ) ) ;
#7878 = AXIS2_PLACEMENT_3D ( 'NONE', #4345, #8049, #1156 ) ;
#7879 = AXIS2_PLACEMENT_3D ( 'NONE', #7621, #6544, #9979 ) ;
#7880 = ORIENTED_EDGE ( 'NONE', *, *, #1250, .F. ) ;
#7881 = AXIS2_PLACEMENT_3D ( 'NONE', #9957, #14606, #13460 ) ;
#7882 = EDGE_CURVE ( 'NONE', #6432, #4604, #12698, .T. ) ;
#7883 = EDGE_LOOP ( 'NONE', ( #1505, #6473, #13195, #10433, #3328 ) ) ;
#7884 = DIRECTION ( 'NONE',  ( 0.000000000000000000, 0.000000000000000000, 1.000000000000000000 ) ) ;
#7885 = VERTEX_POINT ( 'NONE', #12084 ) ;
#7886 = DIRECTION ( 'NONE',  ( 1.000000000000000000, 0.000000000000000000, 0.000000000000000000 ) ) ;
#7887 = DIRECTION ( 'NONE',  ( -0.000000000000000000, -0.000000000000000000, 1.000000000000000000 ) ) ;
#7888 = STYLED_ITEM ( 'NONE', ( #7197 ), #4390 ) ;
#7889 = DIRECTION ( 'NONE',  ( 0.000000000000000000, 0.000000000000000000, 1.000000000000000000 ) ) ;
#7890 = DIRECTION ( 'NONE',  ( -1.000000000000000000, 0.000000000000000000, 0.000000000000000000 ) ) ;
#7891 = DIRECTION ( 'NONE',  ( 1.000000000000000000, 0.000000000000000000, -0.000000000000000000 ) ) ;
#7892 = ORIENTED_EDGE ( 'NONE', *, *, #7474, .F. ) ;
#7893 = DIRECTION ( 'NONE',  ( -1.000000000000000000, 0.000000000000000000, 0.000000000000000000 ) ) ;
#7894 = ORIENTED_EDGE ( 'NONE', *, *, #2545, .T. ) ;
#7895 = CIRCLE ( 'NONE', #10807, 3.000000000000002665 ) ;
#7896 = CARTESIAN_POINT ( 'NONE',  ( -11.55014193876141526, 53.26842454702440222, -8.000000000000000000 ) ) ;
#7897 = DIRECTION ( 'NONE',  ( -0.000000000000000000, -0.000000000000000000, -1.000000000000000000 ) ) ;
#7898 = AXIS2_PLACEMENT_3D ( 'NONE', #3793, #57, #10606 ) ;
#7899 = ORIENTED_EDGE ( 'NONE', *, *, #11022, .T. ) ;
#7900 = LINE ( 'NONE', #14899, #6656 ) ;
#7901 = ORIENTED_EDGE ( 'NONE', *, *, #3663, .F. ) ;
#7902 = CYLINDRICAL_SURFACE ( 'NONE', #5449, 56.99999999999999289 ) ;
#7903 = CARTESIAN_POINT ( 'NONE',  ( 3.999999999999996447, 2.309401076758498039, -3.433295621305378020 ) ) ;
#7904 = CARTESIAN_POINT ( 'NONE',  ( -36.14014761921588104, 11.74264578624790190, -28.00000000000000000 ) ) ;
#7905 = CARTESIAN_POINT ( 'NONE',  ( -11.46932393819253626, 106.3836852522821346, 18.05815993169795064 ) ) ;
#7906 = ADVANCED_FACE ( 'NONE', ( #7208 ), #14278, .T. ) ;
#7907 = LINE ( 'NONE', #2139, #10185 ) ;
#7908 = CONICAL_SURFACE ( 'NONE', #2569, 4.000000000000000000, 0.8911886515913786111 ) ;
#7909 = CARTESIAN_POINT ( 'NONE',  ( 91.27544013909738396, -39.61975340586589311, -13.00000000000000178 ) ) ;
#7910 = FACE_OUTER_BOUND ( 'NONE', #11043, .T. ) ;
#7911 = LINE ( 'NONE', #6690, #294 ) ;
#7912 = VERTEX_POINT ( 'NONE', #14352 ) ;
#7913 = CARTESIAN_POINT ( 'NONE',  ( 0.000000000000000000, 0.000000000000000000, -10.50000000000000000 ) ) ;
#7914 = DIRECTION ( 'NONE',  ( 0.000000000000000000, 0.000000000000000000, 1.000000000000000000 ) ) ;
#7915 = CARTESIAN_POINT ( 'NONE',  ( -25.00000000000000000, 81.24038404635962252, -16.00000000000000000 ) ) ;
#7916 = AXIS2_PLACEMENT_3D ( 'NONE', #13371, #10023, #13515 ) ;
#7917 = PRODUCT ( 'brake disk', 'brake disk', '', ( #4306 ) ) ;
#7918 = DIRECTION ( 'NONE',  ( 0.000000000000000000, 0.000000000000000000, -1.000000000000000000 ) ) ;
#7919 = VERTEX_POINT ( 'NONE', #7282 ) ;
#7920 = CARTESIAN_POINT ( 'NONE',  ( 42.00000000000000711, 81.24038404635960831, 31.00000000000000000 ) ) ;
#7921 = VERTEX_POINT ( 'NONE', #6217 ) ;
#7922 = EDGE_CURVE ( 'NONE', #11359, #1631, #9658, .T. ) ;
#7923 = CARTESIAN_POINT ( 'NONE',  ( 33.29654390035847911, -41.94820822869180432, -10.50000000000000000 ) ) ;
#7924 = EDGE_CURVE ( 'NONE', #7885, #1981, #7232, .T. ) ;
#7925 = SURFACE_SIDE_STYLE ('',( #12274 ) ) ;
#7926 = EDGE_CURVE ( 'NONE', #10396, #9550, #14133, .T. ) ;
#7927 = CARTESIAN_POINT ( 'NONE',  ( 31.47058823529413729, 102.2673069760056563, -79.80561291909842225 ) ) ;
#7928 = CARTESIAN_POINT ( 'NONE',  ( 2.500000000000002220, 2.357898499370430834, -6.938893903907228378E-15 ) ) ;
#7929 = VERTEX_POINT ( 'NONE', #6069 ) ;
#7930 = EDGE_LOOP ( 'NONE', ( #10030, #12112, #226, #8263 ) ) ;
#7931 = ORIENTED_EDGE ( 'NONE', *, *, #1813, .F. ) ;
#7932 = DIRECTION ( 'NONE',  ( 0.000000000000000000, 0.000000000000000000, 1.000000000000000000 ) ) ;
#7933 = LINE ( 'NONE', #13634, #6380 ) ;
#7934 = CYLINDRICAL_SURFACE ( 'NONE', #5149, 59.50000000000000000 ) ;
#7935 = ORIENTED_EDGE ( 'NONE', *, *, #5175, .T. ) ;
#7936 = EDGE_LOOP ( 'NONE', ( #2358, #2227, #14084, #5404, #1662 ) ) ;
#7937 = ORIENTED_EDGE ( 'NONE', *, *, #2480, .F. ) ;
#7938 = CIRCLE ( 'NONE', #11102, 50.00000000000000000 ) ;
#7939 = CARTESIAN_POINT ( 'NONE',  ( 11.92448918074846986, 74.04612619069749258, 17.34622847719485605 ) ) ;
#7940 = CARTESIAN_POINT ( 'NONE',  ( 0.000000000000000000, 4.618802153517009401, -5.000000000000000888 ) ) ;
#7941 = CYLINDRICAL_SURFACE ( 'NONE', #12691, 50.00000000000000000 ) ;
#7942 = LINE ( 'NONE', #10000, #3320 ) ;
#7943 = DIRECTION ( 'NONE',  ( 0.000000000000000000, 1.000000000000000000, -0.000000000000000000 ) ) ;
#7944 = ADVANCED_FACE ( 'NONE', ( #13226 ), #5027, .T. ) ;
#7945 = ORIENTED_EDGE ( 'NONE', *, *, #5188, .F. ) ;
#7946 = DIRECTION ( 'NONE',  ( -1.000000000000000000, 0.000000000000000000, 0.000000000000000000 ) ) ;
#7947 = DIRECTION ( 'NONE',  ( 0.000000000000000000, 0.000000000000000000, 1.000000000000000000 ) ) ;
#7948 = CIRCLE ( 'NONE', #6486, 3.000000000000002665 ) ;
#7949 = EDGE_CURVE ( 'NONE', #10570, #13797, #2817, .T. ) ;
#7950 = ORIENTED_EDGE ( 'NONE', *, *, #14014, .F. ) ;
#7951 = ORIENTED_EDGE ( 'NONE', *, *, #6060, .T. ) ;
#7952 = DIRECTION ( 'NONE',  ( 0.000000000000000000, 0.000000000000000000, -1.000000000000000000 ) ) ;
#7953 = ORIENTED_EDGE ( 'NONE', *, *, #10884, .F. ) ;
#7954 = LINE ( 'NONE', #14883, #2936 ) ;
#7955 = CARTESIAN_POINT ( 'NONE',  ( -13.71740939043329277, 51.19406879332069593, -8.000000000000000000 ) ) ;
#7956 = PLANE ( 'NONE',  #7145 ) ;
#7957 = CARTESIAN_POINT ( 'NONE',  ( -2.807080416178826088, 3.225969019225362722, -3.502507215260544982 ) ) ;
#7958 = EDGE_CURVE ( 'NONE', #2090, #14329, #13076, .T. ) ;
#7959 = FACE_OUTER_BOUND ( 'NONE', #9307, .T. ) ;
#7960 = EDGE_CURVE ( 'NONE', #4919, #4753, #965, .T. ) ;
#7961 = ORIENTED_EDGE ( 'NONE', *, *, #12347, .T. ) ;
#7962 = LINE ( 'NONE', #12604, #6074 ) ;
#7963 = EDGE_LOOP ( 'NONE', ( #7539, #14256, #7880, #13740, #6972 ) ) ;
#7964 = DIRECTION ( 'NONE',  ( 0.000000000000000000, 0.000000000000000000, -1.000000000000000000 ) ) ;
#7965 = CARTESIAN_POINT ( 'NONE',  ( -4.207491450040565795, 2.029819825146467416, -3.671670828759564742 ) ) ;
#7966 = VERTEX_POINT ( 'NONE', #1676 ) ;
#7967 = DIRECTION ( 'NONE',  ( 0.000000000000000000, 0.000000000000000000, 1.000000000000000000 ) ) ;
#7968 = EDGE_CURVE ( 'NONE', #11825, #14730, #3136, .T. ) ;
#7969 = AXIS2_PLACEMENT_3D ( 'NONE', #5994, #10713, #13147 ) ;
#7970 = CARTESIAN_POINT ( 'NONE',  ( 27.94117647058824616, 90.79807628710781842, 23.50000000000000355 ) ) ;
#7971 = ORIENTED_EDGE ( 'NONE', *, *, #12768, .F. ) ;
#7972 = CARTESIAN_POINT ( 'NONE',  ( 3.510273485745305955, 2.827716139362653092, -3.610536846335885564 ) ) ;
#7973 = CARTESIAN_POINT ( 'NONE',  ( 71.58935777509475429, -68.58935777509547904, -8.000000000000000000 ) ) ;
#7974 = DIRECTION ( 'NONE',  ( 1.000000000000000000, 0.000000000000000000, 0.000000000000000000 ) ) ;
#7975 = DIRECTION ( 'NONE',  ( 1.000000000000000000, 0.000000000000000000, -0.000000000000000000 ) ) ;
#7976 = CARTESIAN_POINT ( 'NONE',  ( -3.999999999999634959, -1.658469974638516753, -3.531532913076921076 ) ) ;
#7977 = EDGE_CURVE ( 'NONE', #664, #4586, #2888, .T. ) ;
#7978 = AXIS2_PLACEMENT_3D ( 'NONE', #6670, #11324, #924 ) ;
#7979 = CARTESIAN_POINT ( 'NONE',  ( -6.451868917687557214, -52.36539807335606156, 10.49999999999999822 ) ) ;
#7980 = VERTEX_POINT ( 'NONE', #10858 ) ;
#7981 = LINE ( 'NONE', #1099, #3077 ) ;
#7982 = DIRECTION ( 'NONE',  ( -1.000000000000000000, 0.000000000000000000, 0.000000000000000000 ) ) ;
#7983 = CARTESIAN_POINT ( 'NONE',  ( -56.43380494354004639, -12.86891638962099549, -13.00000000000000178 ) ) ;
#7984 = VERTEX_POINT ( 'NONE', #14214 ) ;
#7985 = AXIS2_PLACEMENT_3D ( 'NONE', #14417, #14341, #6207 ) ;
#7986 = DIRECTION ( 'NONE',  ( 1.000000000000000000, 0.000000000000000000, 0.000000000000000000 ) ) ;
#7987 = EDGE_LOOP ( 'NONE', ( #10714, #2438, #5129, #8586, #12253 ) ) ;
#7988 = DIRECTION ( 'NONE',  ( 0.000000000000000000, 0.000000000000000000, -1.000000000000000000 ) ) ;
#7989 = AXIS2_PLACEMENT_3D ( 'NONE', #11164, #5396, #6587 ) ;
#7990 = ORIENTED_EDGE ( 'NONE', *, *, #3710, .T. ) ;
#7991 = AXIS2_PLACEMENT_3D ( 'NONE', #5086, #2512, #12083 ) ;
#7992 = CARTESIAN_POINT ( 'NONE',  ( -3.355112389629167691, 2.681727112203151631, -0.2256878752776672603 ) ) ;
#7993 = DIRECTION ( 'NONE',  ( 0.000000000000000000, 0.000000000000000000, 1.000000000000000000 ) ) ;
#7994 = CARTESIAN_POINT ( 'NONE',  ( -56.43380494354004639, -12.86891638962099549, 8.000000000000000000 ) ) ;
#7995 = DIRECTION ( 'NONE',  ( 1.000000000000000000, 0.000000000000000000, 0.000000000000000000 ) ) ;
#7996 = ORIENTED_EDGE ( 'NONE', *, *, #62, .F. ) ;
#7997 = ORIENTED_EDGE ( 'NONE', *, *, #14663, .F. ) ;
#7998 = VERTEX_POINT ( 'NONE', #13070 ) ;
#7999 = ORIENTED_EDGE ( 'NONE', *, *, #4087, .F. ) ;
#8000 = AXIS2_PLACEMENT_3D ( 'NONE', #708, #8743, #8896 ) ;
#8001 = EDGE_CURVE ( 'NONE', #2326, #7158, #2327, .T. ) ;
#8002 = DIRECTION ( 'NONE',  ( -0.2941176470588238168, 0.9557692240748187906, -0.000000000000000000 ) ) ;
#8003 = CIRCLE ( 'NONE', #9941, 56.99999999999999289 ) ;
#8004 = CARTESIAN_POINT ( 'NONE',  ( 19.68583958711426263, -30.74264578624780597, 14.49999999999999822 ) ) ;
#8005 = AXIS2_PLACEMENT_3D ( 'NONE', #4560, #4709, #10395 ) ;
#8006 = SHAPE_REPRESENTATION ( 'socket head cap screw_iso_ISO 4762 M5 x 50 - 22N', ( #5108 ), #10652 ) ;
#8007 = DIRECTION ( 'NONE',  ( 0.000000000000000000, 1.000000000000000000, -1.471414886128460880E-15 ) ) ;
#8008 = EDGE_CURVE ( 'NONE', #6463, #13160, #11389, .T. ) ;
#8010 = ORIENTED_EDGE ( 'NONE', *, *, #12667, .F. ) ;
#8009 = ADVANCED_FACE ( 'NONE', ( #6143 ), #10630, .T. ) ;
#8011 = ORIENTED_EDGE ( 'NONE', *, *, #180, .F. ) ;
#8012 = AXIS2_PLACEMENT_3D ( 'NONE', #6361, #11946, #1533 ) ;
#8013 = ORIENTED_EDGE ( 'NONE', *, *, #4407, .T. ) ;
#8014 = AXIS2_PLACEMENT_3D ( 'NONE', #1821, #6436, #11087 ) ;
#8015 = DIRECTION ( 'NONE',  ( -0.000000000000000000, -0.000000000000000000, -1.000000000000000000 ) ) ;
#8016 = EDGE_CURVE ( 'NONE', #1144, #10864, #8940, .T. ) ;
#8017 = VECTOR ( 'NONE', #14212, 1000.000000000000000 ) ;
#8018 = CARTESIAN_POINT ( 'NONE',  ( 44.89637028918153305, 5.498219616798048790E-15, 14.49999999999999822 ) ) ;
#8019 = CIRCLE ( 'NONE', #13855, 53.55662432702593634 ) ;
#8020 = DIRECTION ( 'NONE',  ( 0.000000000000000000, 1.224646799147353207E-16, 1.000000000000000000 ) ) ;
#8021 = DIRECTION ( 'NONE',  ( -1.000000000000000000, 0.000000000000000000, 0.000000000000000000 ) ) ;
#8022 = ORIENTED_EDGE ( 'NONE', *, *, #12540, .F. ) ;
#8023 = DIRECTION ( 'NONE',  ( 0.000000000000000000, 0.000000000000000000, 1.000000000000000000 ) ) ;
#8024 = ORIENTED_EDGE ( 'NONE', *, *, #8420, .T. ) ;
#8025 = EDGE_CURVE ( 'NONE', #4530, #9553, #12834, .T. ) ;
#8026 = DIRECTION ( 'NONE',  ( 0.000000000000000000, 0.000000000000000000, -1.000000000000000000 ) ) ;
#8027 = CARTESIAN_POINT ( 'NONE',  ( -27.94117647058823550, 90.79807628710781842, 23.50000000000000355 ) ) ;
#8028 = CIRCLE ( 'NONE', #1017, 0.5000000000000004441 ) ;
#8029 = ADVANCED_FACE ( 'NONE', ( #621 ), #7665, .F. ) ;
#8030 = VERTEX_POINT ( 'NONE', #11012 ) ;
#8031 = AXIS2_PLACEMENT_3D ( 'NONE', #3778, #3470, #10374 ) ;
#8032 = VERTEX_POINT ( 'NONE', #691 ) ;
#8033 = CARTESIAN_POINT ( 'NONE',  ( -45.89934640057513349, 26.50000000000019540, 8.000000000000000000 ) ) ;
#8034 = ORIENTED_EDGE ( 'NONE', *, *, #853, .F. ) ;
#8035 = ORIENTED_EDGE ( 'NONE', *, *, #4462, .T. ) ;
#8036 = LINE ( 'NONE', #12593, #9471 ) ;
#8037 = CARTESIAN_POINT ( 'NONE',  ( 9.706953719245472456, 57.06275842387054098, -10.50000000000000000 ) ) ;
#8038 = CIRCLE ( 'NONE', #1501, 53.55662432702593634 ) ;
#8039 = CARTESIAN_POINT ( 'NONE',  ( -33.49014761921589667, 11.74264578624790190, -25.50000000000000355 ) ) ;
#8040 = DIRECTION ( 'NONE',  ( 0.000000000000000000, 0.5000000000000008882, 0.8660254037844381525 ) ) ;
#8041 = ORIENTED_EDGE ( 'NONE', *, *, #8804, .F. ) ;
#8042 = CYLINDRICAL_SURFACE ( 'NONE', #9193, 2.649999999999985700 ) ;
#8043 = VECTOR ( 'NONE', #6703, 1000.000000000000000 ) ;
#8044 = EDGE_LOOP ( 'NONE', ( #14776, #7566, #14413, #3387 ) ) ;
#8045 =( REPRESENTATION_RELATIONSHIP ('NONE','NONE', #12187, #10623 ) REPRESENTATION_RELATIONSHIP_WITH_TRANSFORMATION ( #3157 )SHAPE_REPRESENTATION_RELATIONSHIP( ) );
#8046 = DIRECTION ( 'NONE',  ( 1.000000000000000000, 0.000000000000000000, -0.000000000000000000 ) ) ;
#8047 = AXIS2_PLACEMENT_3D ( 'NONE', #2225, #6839, #1233 ) ;
#8048 = ORIENTED_EDGE ( 'NONE', *, *, #13743, .T. ) ;
#8049 = DIRECTION ( 'NONE',  ( -0.000000000000000000, -0.000000000000000000, -1.000000000000000000 ) ) ;
#8050 = ORIENTED_EDGE ( 'NONE', *, *, #13125, .F. ) ;
#8051 = ADVANCED_FACE ( 'NONE', ( #11091 ), #9908, .F. ) ;
#8052 = CARTESIAN_POINT ( 'NONE',  ( -13.21740939043329099, 51.19406879332069593, 10.49999999999999822 ) ) ;
#8053 = EDGE_CURVE ( 'NONE', #12802, #8108, #2400, .T. ) ;
#8054 = ORIENTED_EDGE ( 'NONE', *, *, #3102, .T. ) ;
#8055 = DIRECTION ( 'NONE',  ( 0.000000000000000000, 0.000000000000000000, 1.000000000000000000 ) ) ;
#8056 = EDGE_CURVE ( 'NONE', #8030, #6492, #5307, .T. ) ;
#8057 = PLANE ( 'NONE',  #10301 ) ;
#8058 = CARTESIAN_POINT ( 'NONE',  ( 35.00000000000000000, 81.24038404635960831, -23.50000000000000000 ) ) ;
#8059 = DIRECTION ( 'NONE',  ( -1.000000000000000000, 0.000000000000000000, 0.000000000000000000 ) ) ;
#8060 = CARTESIAN_POINT ( 'NONE',  ( 45.88839665196118744, -26.99988008862642630, -10.50000000000000000 ) ) ;
#8061 = CIRCLE ( 'NONE', #9998, 14.00000000000000000 ) ;
#8062 = EDGE_CURVE ( 'NONE', #12788, #9888, #12377, .T. ) ;
#8063 = DIRECTION ( 'NONE',  ( 0.000000000000000000, 0.000000000000000000, -1.000000000000000000 ) ) ;
#8064 = EDGE_LOOP ( 'NONE', ( #2339, #959, #4671, #7822 ) ) ;
#8065 = CIRCLE ( 'NONE', #10731, 5.384454397937118664 ) ;
#8066 = CYLINDRICAL_SURFACE ( 'NONE', #5018, 0.5000000000000004441 ) ;
#8067 = CYLINDRICAL_SURFACE ( 'NONE', #12958, 3.000000000000004441 ) ;
#8068 = DIRECTION ( 'NONE',  ( 0.000000000000000000, 0.000000000000000000, 1.000000000000000000 ) ) ;
#8069 = DIRECTION ( 'NONE',  ( 0.000000000000000000, 0.000000000000000000, 1.000000000000000000 ) ) ;
#8070 = EDGE_CURVE ( 'NONE', #9479, #7296, #2644, .T. ) ;
#8071 = ORIENTED_EDGE ( 'NONE', *, *, #13833, .F. ) ;
#8072 = DIRECTION ( 'NONE',  ( -1.000000000000000000, 0.000000000000000000, 0.000000000000000000 ) ) ;
#8073 = VERTEX_POINT ( 'NONE', #1971 ) ;
#8074 = AXIS2_PLACEMENT_3D ( 'NONE', #12026, #9638, #1537 ) ;
#8075 = DIRECTION ( 'NONE',  ( -0.000000000000000000, -0.000000000000000000, 1.000000000000000000 ) ) ;
#8076 = LINE ( 'NONE', #3534, #13400 ) ;
#8077 = CARTESIAN_POINT ( 'NONE',  ( 38.26834323650905390, 92.38795325112863566, 8.000000000000000000 ) ) ;
#8078 = CARTESIAN_POINT ( 'NONE',  ( 12.86891638962116247, -56.43380494354001087, -8.000000000000000000 ) ) ;
#8079 = ORIENTED_EDGE ( 'NONE', *, *, #2398, .F. ) ;
#8080 = VECTOR ( 'NONE', #8328, 1000.000000000000000 ) ;
#8081 = DIRECTION ( 'NONE',  ( 0.000000000000000000, 0.000000000000000000, 1.000000000000000000 ) ) ;
#8082 = DIRECTION ( 'NONE',  ( 0.000000000000000000, 0.000000000000000000, 1.000000000000000000 ) ) ;
#8083 = LINE ( 'NONE', #4603, #2731 ) ;
#8084 = ORIENTED_EDGE ( 'NONE', *, *, #7958, .F. ) ;
#8085 = VECTOR ( 'NONE', #4973, 1000.000000000000000 ) ;
#8086 = ORIENTED_EDGE ( 'NONE', *, *, #3201, .F. ) ;
#8087 = ORIENTED_EDGE ( 'NONE', *, *, #3838, .T. ) ;
#8088 = CARTESIAN_POINT ( 'NONE',  ( 7.500000000000000000, 74.62405778299650194, 20.00000000000000000 ) ) ;
#8089 = CARTESIAN_POINT ( 'NONE',  ( 6.917888187663118416, 52.54657765281190507, 8.000000000000000000 ) ) ;
#8090 = CYLINDRICAL_SURFACE ( 'NONE', #3483, 107.0000000000000284 ) ;
#8091 = EDGE_CURVE ( 'NONE', #7240, #8815, #6508, .T. ) ;
#8092 = DIRECTION ( 'NONE',  ( -1.000000000000000000, 0.000000000000000000, 0.000000000000000000 ) ) ;
#8093 = CIRCLE ( 'NONE', #3990, 0.5000000000000073275 ) ;
#8094 = AXIS2_PLACEMENT_3D ( 'NONE', #10364, #4673, #12865 ) ;
#8095 = CIRCLE ( 'NONE', #4023, 0.5000000000000043299 ) ;
#8096 = EDGE_CURVE ( 'NONE', #6738, #11326, #12123, .T. ) ;
#8097 = CIRCLE ( 'NONE', #8820, 2.649999999999985700 ) ;
#8098 = CYLINDRICAL_SURFACE ( 'NONE', #2211, 100.0000000000000000 ) ;
#8099 = VERTEX_POINT ( 'NONE', #8946 ) ;
#8100 = SHAPE_REPRESENTATION ( 'brake disk', ( #5108 ), #6780 ) ;
#8101 = DIRECTION ( 'NONE',  ( -1.000000000000000000, 0.000000000000000000, 0.000000000000000000 ) ) ;
#8102 = CARTESIAN_POINT ( 'NONE',  ( 57.06275842387049835, -9.706953719245678514, 10.49999999999999822 ) ) ;
#8103 = B_SPLINE_CURVE_WITH_KNOTS ( 'NONE', 3,
 ( #11494, #12838, #12696, #11713, #1305, #1226, #3355, #5923, #9408, #4649, #9269, #3285, #7905, #2362, #13921, #4573, #1091, #2138, #6751, #10339 ),
 .UNSPECIFIED., .F., .F.,
 ( 4, 2, 2, 2, 2, 2, 2, 2, 2, 4 ),
 ( 8.673617379884035472E-19, 0.0009783702772842232508, 0.001467555415926338454, 0.001956740554568453874, 0.002935110831852691653, 0.003913481109136930300, 0.004891851386421167645, 0.005870221663705405858, 0.006848591940989644071, 0.007826962218273881416 ),
 .UNSPECIFIED. ) ;
#8104 = ORIENTED_EDGE ( 'NONE', *, *, #2820, .F. ) ;
#8105 = ORIENTED_EDGE ( 'NONE', *, *, #5634, .T. ) ;
#8106 = DIRECTION ( 'NONE',  ( 0.000000000000000000, 0.000000000000000000, -1.000000000000000000 ) ) ;
#8107 = CIRCLE ( 'NONE', #1569, 63.00000000000000000 ) ;
#8108 = VERTEX_POINT ( 'NONE', #7584 ) ;
#8109 = ORIENTED_EDGE ( 'NONE', *, *, #6242, .T. ) ;
#8110 = EDGE_CURVE ( 'NONE', #7623, #7147, #6041, .T. ) ;
#8111 = CARTESIAN_POINT ( 'NONE',  ( 26.49999999999971578, 45.89934640057541060, -10.50000000000000000 ) ) ;
#8112 = CARTESIAN_POINT ( 'NONE',  ( -3.999999999999996447, 2.309401076758498039, -3.433295621305378020 ) ) ;
#8113 = DIRECTION ( 'NONE',  ( 0.000000000000000000, 0.000000000000000000, 1.000000000000000000 ) ) ;
#8114 = CARTESIAN_POINT ( 'NONE',  ( -4.141042297810613171, 2.227970268150412991, -3.687027686973620266 ) ) ;
#8115 = ADVANCED_FACE ( 'NONE', ( #1826 ), #14812, .F. ) ;
#8116 = ADVANCED_FACE ( 'NONE', ( #4268 ), #9438, .T. ) ;
#8117 = AXIS2_PLACEMENT_3D ( 'NONE', #3220, #8550, #1727 ) ;
#8118 = CARTESIAN_POINT ( 'NONE',  ( 99.48933418828643482, -1.674280531759671620, -13.00000000000000178 ) ) ;
#8119 = ORIENTED_EDGE ( 'NONE', *, *, #5535, .T. ) ;
#8120 = CIRCLE ( 'NONE', #10058, 59.50000000000000000 ) ;
#8121 = AXIS2_PLACEMENT_3D ( 'NONE', #6537, #714, #13611 ) ;
#8122 = CARTESIAN_POINT ( 'NONE',  ( 53.20607447915237742, -6.117650515114167575, -10.50000000000000000 ) ) ;
#8123 = VECTOR ( 'NONE', #9407, 1000.000000000000000 ) ;
#8124 = CARTESIAN_POINT ( 'NONE',  ( 30.80502811811196295, 49.00442420936003174, -13.00000000000000178 ) ) ;
#8125 = ORIENTED_EDGE ( 'NONE', *, *, #3013, .T. ) ;
#8126 = DIRECTION ( 'NONE',  ( 1.000000000000000000, 0.000000000000000000, 0.000000000000000000 ) ) ;
#8127 = ORIENTED_EDGE ( 'NONE', *, *, #2736, .T. ) ;
#8128 = CIRCLE ( 'NONE', #2314, 0.5000000000000073275 ) ;
#8129 = CARTESIAN_POINT ( 'NONE',  ( 30.68146655995342087, 96.22723358344990174, 14.04702900388066844 ) ) ;
#8130 = ORIENTED_EDGE ( 'NONE', *, *, #8485, .F. ) ;
#8131 = CARTESIAN_POINT ( 'NONE',  ( -9.703618315745389467, 62.24871376222712627, 19.49715125027359974 ) ) ;
#8132 = AXIS2_PLACEMENT_3D ( 'NONE', #4847, #13750, #3339 ) ;
#8133 = CARTESIAN_POINT ( 'NONE',  ( -5.560781378645573980, 0.000000000000000000, -4.000000000000000000 ) ) ;
#8134 = CARTESIAN_POINT ( 'NONE',  ( 31.47058823529413374, 102.2673069760056563, 26.00000000000000000 ) ) ;
#8135 = FACE_OUTER_BOUND ( 'NONE', #7006, .T. ) ;
#8136 = DIRECTION ( 'NONE',  ( 1.000000000000000000, 0.000000000000000000, 0.000000000000000000 ) ) ;
#8137 = ITEM_DEFINED_TRANSFORMATION ( 'NONE', 'NONE', #7000,  #5108 ) ;
#8138 = VECTOR ( 'NONE', #7013, 1000.000000000000000 ) ;
#8139 = DIRECTION ( 'NONE',  ( 0.000000000000000000, 0.000000000000000000, 1.000000000000000000 ) ) ;
#8140 = AXIS2_PLACEMENT_3D ( 'NONE', #5466, #7952, #7804 ) ;
#8141 = ORIENTED_EDGE ( 'NONE', *, *, #12138, .T. ) ;
#8142 = EDGE_CURVE ( 'NONE', #3633, #14620, #2902, .T. ) ;
#8143 = DIRECTION ( 'NONE',  ( -0.000000000000000000, 1.000000000000000000, -0.000000000000000000 ) ) ;
#8144 = LINE ( 'NONE', #2369, #3963 ) ;
#8145 = EDGE_CURVE ( 'NONE', #12042, #9441, #3192, .T. ) ;
#8146 = CARTESIAN_POINT ( 'NONE',  ( 89.61631465359491244, 37.12029293941346708, -10.50000000000000000 ) ) ;
#8147 = PLANE ( 'NONE',  #6399 ) ;
#8148 = ORIENTED_EDGE ( 'NONE', *, *, #5461, .T. ) ;
#8149 = AXIS2_PLACEMENT_3D ( 'NONE', #11595, #6860, #3236 ) ;
#8150 = EDGE_CURVE ( 'NONE', #5144, #14931, #9919, .T. ) ;
#8151 = DIRECTION ( 'NONE',  ( 1.000000000000000000, 0.000000000000000000, 0.000000000000000000 ) ) ;
#8152 = VERTEX_POINT ( 'NONE', #9937 ) ;
#8153 = CARTESIAN_POINT ( 'NONE',  ( -52.54657765281192638, 6.917888187662934563, -13.00000000000000178 ) ) ;
#8154 = DIRECTION ( 'NONE',  ( 0.000000000000000000, 0.000000000000000000, 1.000000000000000000 ) ) ;
#8155 = DIRECTION ( 'NONE',  ( 1.000000000000000000, 0.000000000000000000, 0.000000000000000000 ) ) ;
#8156 = CARTESIAN_POINT ( 'NONE',  ( -9.706953719245875689, -57.06275842387046993, -8.000000000000000000 ) ) ;
#8157 = EDGE_CURVE ( 'NONE', #1607, #900, #11877, .T. ) ;
#8158 = ORIENTED_EDGE ( 'NONE', *, *, #3691, .F. ) ;
#8159 = EDGE_CURVE ( 'NONE', #11131, #7351, #3635, .T. ) ;
#8160 = AXIS2_PLACEMENT_3D ( 'NONE', #14837, #9637, #9569 ) ;
#8161 = CARTESIAN_POINT ( 'NONE',  ( 46.24878538001313188, -27.00670028307179749, -10.50000000000000000 ) ) ;
#8162 = CARTESIAN_POINT ( 'NONE',  ( 0.000000000000000000, 0.000000000000000000, -28.00000000000000000 ) ) ;
#8163 = DIRECTION ( 'NONE',  ( 0.000000000000000000, 0.000000000000000000, 1.000000000000000000 ) ) ;
#8164 = VERTEX_POINT ( 'NONE', #1213 ) ;
#8165 = ORIENTED_EDGE ( 'NONE', *, *, #4343, .F. ) ;
#8166 = EDGE_CURVE ( 'NONE', #9519, #11532, #9178, .T. ) ;
#8167 = ORIENTED_EDGE ( 'NONE', *, *, #2260, .T. ) ;
#8168 = DIRECTION ( 'NONE',  ( 1.000000000000000000, 0.000000000000000000, 0.000000000000000000 ) ) ;
#8169 = LINE ( 'NONE', #11604, #1729 ) ;
#8170 = CARTESIAN_POINT ( 'NONE',  ( 69.20695371924547601, 57.06275842387054098, -10.50000000000000000 ) ) ;
#8171 = DIRECTION ( 'NONE',  ( 1.000000000000000000, 0.000000000000000000, 0.000000000000000000 ) ) ;
#8172 = VERTEX_POINT ( 'NONE', #3420 ) ;
#8173 = CARTESIAN_POINT ( 'NONE',  ( 39.30189486418243661, 33.47282819776626894, 8.000000000000000000 ) ) ;
#8174 = EDGE_LOOP ( 'NONE', ( #9381, #2261, #9691, #1803 ) ) ;
#8175 = ORIENTED_EDGE ( 'NONE', *, *, #4618, .F. ) ;
#8176 = ORIENTED_EDGE ( 'NONE', *, *, #91, .F. ) ;
#8177 = FACE_OUTER_BOUND ( 'NONE', #10535, .T. ) ;
#8178 = FACE_OUTER_BOUND ( 'NONE', #3791, .T. ) ;
#8179 = EDGE_LOOP ( 'NONE', ( #14529, #13325, #11155, #2718, #5463 ) ) ;
#8180 = VERTEX_POINT ( 'NONE', #5833 ) ;
#8181 = DIRECTION ( 'NONE',  ( 0.000000000000000000, 0.000000000000000000, 1.000000000000000000 ) ) ;
#8182 = ORIENTED_EDGE ( 'NONE', *, *, #10699, .T. ) ;
#8183 = ORIENTED_EDGE ( 'NONE', *, *, #9893, .F. ) ;
#8184 = DIRECTION ( 'NONE',  ( 1.000000000000000000, 0.000000000000000000, 0.000000000000000000 ) ) ;
#8185 = CARTESIAN_POINT ( 'NONE',  ( 0.000000000000000000, 0.000000000000000000, 8.000000000000000000 ) ) ;
#8186 = DIRECTION ( 'NONE',  ( 1.000000000000000000, 0.000000000000000000, 0.000000000000000000 ) ) ;
#8187 = CARTESIAN_POINT ( 'NONE',  ( -52.04657765281192638, 6.917888187662934563, 10.49999999999999822 ) ) ;
#8188 = ORIENTED_EDGE ( 'NONE', *, *, #3543, .F. ) ;
#8189 = CARTESIAN_POINT ( 'NONE',  ( -8.914534555419061590, 74.46880876796768689, -19.80411369943039901 ) ) ;
#8190 = LINE ( 'NONE', #68, #719 ) ;
#8191 = ORIENTED_EDGE ( 'NONE', *, *, #6799, .T. ) ;
#8192 = DIRECTION ( 'NONE',  ( -0.000000000000000000, -0.000000000000000000, -1.000000000000000000 ) ) ;
#8193 = ADVANCED_FACE ( 'NONE', ( #11393 ), #12683, .T. ) ;
#8194 = FACE_OUTER_BOUND ( 'NONE', #14280, .T. ) ;
#8195 = EDGE_CURVE ( 'NONE', #3842, #8710, #8190, .T. ) ;
#8196 = VERTEX_POINT ( 'NONE', #5906 ) ;
#8197 = ADVANCED_FACE ( 'NONE', ( #4784 ), #8042, .F. ) ;
#8198 = ADVANCED_FACE ( 'NONE', ( #995 ), #475, .T. ) ;
#8199 = EDGE_LOOP ( 'NONE', ( #1028, #10584, #8720, #8578 ) ) ;
#8200 = CARTESIAN_POINT ( 'NONE',  ( 30.33578517098777638, 96.33676874097987763, 13.50363573142180940 ) ) ;
#8201 = CARTESIAN_POINT ( 'NONE',  ( -42.04772703543551415, -32.26435573746212526, -10.50000000000000000 ) ) ;
#8202 = CARTESIAN_POINT ( 'NONE',  ( 24.98583958711423492, -30.74264578624780597, -25.50000000000000355 ) ) ;
#8203 = CARTESIAN_POINT ( 'NONE',  ( 0.000000000000000000, 0.000000000000000000, -8.000000000000000000 ) ) ;
#8204 = CARTESIAN_POINT ( 'NONE',  ( 0.000000000000000000, 0.000000000000000000, -16.00000000000000000 ) ) ;
#8205 = AXIS2_PLACEMENT_3D ( 'NONE', #4499, #5839, #6821 ) ;
#8206 = CARTESIAN_POINT ( 'NONE',  ( -3.999999999999998224, 1.700094919196804666, -3.320312364301445385 ) ) ;
#8207 = CONTEXT_DEPENDENT_SHAPE_REPRESENTATION ( #12710, #13615 ) ;
#8208 = DIRECTION ( 'NONE',  ( -0.000000000000000000, 1.000000000000000000, -0.000000000000000000 ) ) ;
#8209 = ORIENTED_EDGE ( 'NONE', *, *, #7536, .F. ) ;
#8210 = CARTESIAN_POINT ( 'NONE',  ( -7.500000000000000888, 106.7368258849775202, -20.00000000000000000 ) ) ;
#8211 = CARTESIAN_POINT ( 'NONE',  ( 19.68583958711426263, -30.74264578624780597, -25.50000000000000355 ) ) ;
#8212 = CARTESIAN_POINT ( 'NONE',  ( 0.000000000000000000, 0.000000000000000000, -10.50000000000000000 ) ) ;
#8213 = DIRECTION ( 'NONE',  ( 0.000000000000000000, 0.000000000000000000, -1.000000000000000000 ) ) ;
#8214 = VERTEX_POINT ( 'NONE', #14888 ) ;
#8215 = DIRECTION ( 'NONE',  ( -0.000000000000000000, -0.000000000000000000, 1.000000000000000000 ) ) ;
#8216 = ORIENTED_EDGE ( 'NONE', *, *, #10102, .T. ) ;
#8217 = EDGE_CURVE ( 'NONE', #9064, #14934, #3150, .T. ) ;
#8218 = DIRECTION ( 'NONE',  ( 0.000000000000000000, 0.000000000000000000, 1.000000000000000000 ) ) ;
#8219 = FACE_OUTER_BOUND ( 'NONE', #6621, .T. ) ;
#8220 = VECTOR ( 'NONE', #3440, 1000.000000000000000 ) ;
#8221 = DIRECTION ( 'NONE',  ( 0.000000000000000000, 0.000000000000000000, 1.000000000000000000 ) ) ;
#8222 = FACE_OUTER_BOUND ( 'NONE', #3674, .T. ) ;
#8223 = ORIENTED_EDGE ( 'NONE', *, *, #3939, .T. ) ;
#8224 = ORIENTED_EDGE ( 'NONE', *, *, #4187, .F. ) ;
#8225 = ORIENTED_EDGE ( 'NONE', *, *, #5748, .F. ) ;
#8226 = DIRECTION ( 'NONE',  ( 0.000000000000000000, 0.000000000000000000, 1.000000000000000000 ) ) ;
#8227 = DIRECTION ( 'NONE',  ( 0.000000000000000000, 0.000000000000000000, -1.000000000000000000 ) ) ;
#8228 = DIRECTION ( 'NONE',  ( 0.000000000000000000, 0.000000000000000000, -1.000000000000000000 ) ) ;
#8229 = ORIENTED_EDGE ( 'NONE', *, *, #5827, .F. ) ;
#8230 = CIRCLE ( 'NONE', #10168, 3.000000000000002665 ) ;
#8231 = ORIENTED_EDGE ( 'NONE', *, *, #12994, .T. ) ;
#8232 = ADVANCED_FACE ( 'NONE', ( #7959 ), #6896, .F. ) ;
#8233 = ORIENTED_EDGE ( 'NONE', *, *, #4515, .T. ) ;
#8234 = EDGE_CURVE ( 'NONE', #5947, #11955, #6275, .T. ) ;
#8235 = DIRECTION ( 'NONE',  ( 1.000000000000000000, 0.000000000000000000, 0.000000000000000000 ) ) ;
#8236 = CARTESIAN_POINT ( 'NONE',  ( -68.58935777509570642, -68.58935777509452691, 8.000000000000000000 ) ) ;
#8237 = DIRECTION ( 'NONE',  ( 0.000000000000000000, 0.000000000000000000, -1.000000000000000000 ) ) ;
#8238 = DIRECTION ( 'NONE',  ( 0.000000000000000000, 0.000000000000000000, 1.000000000000000000 ) ) ;
#8239 = AXIS2_PLACEMENT_3D ( 'NONE', #10582, #10358, #4668 ) ;
#8240 = LINE ( 'NONE', #124, #2811 ) ;
#8241 = VECTOR ( 'NONE', #4666, 1000.000000000000000 ) ;
#8242 = ORIENTED_EDGE ( 'NONE', *, *, #5517, .T. ) ;
#8243 = CARTESIAN_POINT ( 'NONE',  ( -8.072481656125564342, 94.65682832148054615, 19.97535367358595693 ) ) ;
#8244 = ORIENTED_EDGE ( 'NONE', *, *, #12023, .F. ) ;
#8245 = AXIS2_PLACEMENT_3D ( 'NONE', #3882, #2740, #9562 ) ;
#8246 = EDGE_CURVE ( 'NONE', #6195, #5327, #14791, .T. ) ;
#8247 = CARTESIAN_POINT ( 'NONE',  ( 50.00000000000000000, -6.123233995736766085E-15, -8.000000000000000000 ) ) ;
#8248 = CARTESIAN_POINT ( 'NONE',  ( 14.07862063237891981, -50.84834283436993729, -10.50000000000000000 ) ) ;
#8249 = CYLINDRICAL_SURFACE ( 'NONE', #3972, 59.50000000000000711 ) ;
#8250 = VERTEX_POINT ( 'NONE', #11478 ) ;
#8251 = CIRCLE ( 'NONE', #13837, 63.00000000000000000 ) ;
#8252 = VERTEX_POINT ( 'NONE', #13982 ) ;
#8253 = CARTESIAN_POINT ( 'NONE',  ( -52.54657765281192638, 6.917888187662934563, -10.50000000000000000 ) ) ;
#8254 = AXIS2_PLACEMENT_3D ( 'NONE', #1449, #2511, #13223 ) ;
#8255 = VERTEX_POINT ( 'NONE', #3573 ) ;
#8256 = ADVANCED_FACE ( 'NONE', ( #5688 ), #10325, .F. ) ;
#8257 = CIRCLE ( 'NONE', #2683, 52.50000000000000711 ) ;
#8258 = DIRECTION ( 'NONE',  ( -0.000000000000000000, -0.000000000000000000, -1.000000000000000000 ) ) ;
#8259 = CARTESIAN_POINT ( 'NONE',  ( -38.79014761921587251, 11.74264578624790190, -25.50000000000000355 ) ) ;
#8260 = CARTESIAN_POINT ( 'NONE',  ( -44.79355920668832880, -31.05588327715819474, 8.000000000000000000 ) ) ;
#8261 = PRESENTATION_STYLE_ASSIGNMENT (( #3942 ) ) ;
#8262 = VECTOR ( 'NONE', #14970, 1000.000000000000000 ) ;
#8263 = ORIENTED_EDGE ( 'NONE', *, *, #5197, .T. ) ;
#8265 = VECTOR ( 'NONE', #13899, 1000.000000000000000 ) ;
#8264 = CARTESIAN_POINT ( 'NONE',  ( -11.92448918074847342, 74.04612619069749258, -17.34622847719484540 ) ) ;
#8266 = DIRECTION ( 'NONE',  ( 1.000000000000000000, 0.000000000000000000, 0.000000000000000000 ) ) ;
#8267 = ORIENTED_EDGE ( 'NONE', *, *, #382, .T. ) ;
#8268 = AXIS2_PLACEMENT_3D ( 'NONE', #3247, #906, #1749 ) ;
#8269 = ORIENTED_EDGE ( 'NONE', *, *, #1380, .T. ) ;
#8270 = VECTOR ( 'NONE', #10915, 1000.000000000000000 ) ;
#8271 = ORIENTED_EDGE ( 'NONE', *, *, #11094, .T. ) ;
#8272 = CARTESIAN_POINT ( 'NONE',  ( 2.278234631210864708E-15, -4.736529461166055555, -3.681130640444385094 ) ) ;
#8273 = AXIS2_PLACEMENT_3D ( 'NONE', #5746, #10228, #2262 ) ;
#8274 = CARTESIAN_POINT ( 'NONE',  ( -3.999999999999996447, -2.309401076758511806, -3.433295621305381573 ) ) ;
#8275 = ORIENTED_EDGE ( 'NONE', *, *, #4089, .F. ) ;
#8276 = DIRECTION ( 'NONE',  ( -0.000000000000000000, -0.000000000000000000, 1.000000000000000000 ) ) ;
#8277 = AXIS2_PLACEMENT_3D ( 'NONE', #12634, #10050, #5427 ) ;
#8278 = DIRECTION ( 'NONE',  ( 1.000000000000000000, 0.000000000000000000, -0.000000000000000000 ) ) ;
#8279 = CARTESIAN_POINT ( 'NONE',  ( 7.500000000000000888, 62.55197838597913318, -20.00000000000000000 ) ) ;
#8280 = CARTESIAN_POINT ( 'NONE',  ( -33.48561063518626923, 47.21331623427104063, -10.50000000000000000 ) ) ;
#8281 = CARTESIAN_POINT ( 'NONE',  ( -4.204114297095385311, 1.660363174096626260, -3.602136431857864807 ) ) ;
#8282 = CONTEXT_DEPENDENT_SHAPE_REPRESENTATION ( #12221, #11198 ) ;
#8283 = ORIENTED_EDGE ( 'NONE', *, *, #1979, .F. ) ;
#8284 = EDGE_CURVE ( 'NONE', #14147, #571, #1454, .T. ) ;
#8285 = DIRECTION ( 'NONE',  ( 1.000000000000000000, 0.000000000000000000, 0.000000000000000000 ) ) ;
#8286 = EDGE_CURVE ( 'NONE', #8164, #11873, #4636, .T. ) ;
#8287 = AXIS2_PLACEMENT_3D ( 'NONE', #2143, #3214, #794 ) ;
#8288 = ORIENTED_EDGE ( 'NONE', *, *, #9078, .F. ) ;
#8289 = PLANE ( 'NONE',  #5731 ) ;
#8290 = DIRECTION ( 'NONE',  ( -1.000000000000000000, 0.000000000000000000, 0.000000000000000000 ) ) ;
#8291 = CIRCLE ( 'NONE', #12180, 3.000000000000002665 ) ;
#8292 = DIRECTION ( 'NONE',  ( 1.000000000000000000, 0.000000000000000000, 0.000000000000000000 ) ) ;
#8293 = DIRECTION ( 'NONE',  ( 0.000000000000000000, -0.4999999999999997780, 0.8660254037844388186 ) ) ;
#8294 = ORIENTED_EDGE ( 'NONE', *, *, #13350, .T. ) ;
#8295 = DIRECTION ( 'NONE',  ( -0.000000000000000000, -0.000000000000000000, 1.000000000000000000 ) ) ;
#8296 = EDGE_LOOP ( 'NONE', ( #13550, #11767, #445, #6375, #5051 ) ) ;
#8297 = AXIS2_PLACEMENT_3D ( 'NONE', #1802, #13555, #3166 ) ;
#8298 = ORIENTED_EDGE ( 'NONE', *, *, #344, .T. ) ;
#8299 = EDGE_CURVE ( 'NONE', #11315, #5870, #8230, .T. ) ;
#8300 = DIRECTION ( 'NONE',  ( 0.000000000000000000, 0.000000000000000000, 1.000000000000000000 ) ) ;
#8301 = CARTESIAN_POINT ( 'NONE',  ( -68.58935777509570642, -68.58935777509452691, -13.00000000000000178 ) ) ;
#8302 = CYLINDRICAL_SURFACE ( 'NONE', #9679, 0.5000000000000043299 ) ;
#8303 = CIRCLE ( 'NONE', #54, 63.00000000000000000 ) ;
#8304 = DIRECTION ( 'NONE',  ( 0.000000000000000000, 0.000000000000000000, 1.000000000000000000 ) ) ;
#8305 = EDGE_CURVE ( 'NONE', #8402, #1144, #14043, .T. ) ;
#8306 = ORIENTED_EDGE ( 'NONE', *, *, #14856, .F. ) ;
#8307 = FACE_OUTER_BOUND ( 'NONE', #10477, .T. ) ;
#8308 = FACE_OUTER_BOUND ( 'NONE', #6643, .T. ) ;
#8309 = AXIS2_PLACEMENT_3D ( 'NONE', #2304, #11585, #5780 ) ;
#8310 = DIRECTION ( 'NONE',  ( -0.000000000000000000, -0.000000000000000000, 1.000000000000000000 ) ) ;
#8311 = EDGE_LOOP ( 'NONE', ( #12766, #4529, #10960, #740 ) ) ;
#8312 = ORIENTED_EDGE ( 'NONE', *, *, #4329, .F. ) ;
#8313 = VECTOR ( 'NONE', #10375, 1000.000000000000000 ) ;
#8314 = ORIENTED_EDGE ( 'NONE', *, *, #1390, .F. ) ;
#8315 = DIRECTION ( 'NONE',  ( 0.000000000000000000, 0.000000000000000000, 1.000000000000000000 ) ) ;
#8316 = DIRECTION ( 'NONE',  ( 1.000000000000000000, 0.000000000000000000, 0.000000000000000000 ) ) ;
#8317 = CARTESIAN_POINT ( 'NONE',  ( 37.12029293941379393, 89.61631465359479876, -8.000000000000000000 ) ) ;
#8318 = SHAPE_REPRESENTATION_RELATIONSHIP ( 'NONE' , 'NONE' ,  #8006, #6552 ) ;
#8319 = CARTESIAN_POINT ( 'NONE',  ( -25.00000000000000000, 81.24038404635962252, -13.50000000000000178 ) ) ;
#8320 = ORIENTED_EDGE ( 'NONE', *, *, #14291, .F. ) ;
#8321 = EDGE_LOOP ( 'NONE', ( #4623, #1062, #8050, #6413, #13188, #3601 ) ) ;
#8322 = EDGE_CURVE ( 'NONE', #479, #2325, #10545, .T. ) ;
#8323 = CARTESIAN_POINT ( 'NONE',  ( 3.000000000000004885, -97.00000000000000000, -8.000000000000000000 ) ) ;
#8325 = EDGE_CURVE ( 'NONE', #11061, #8180, #5613, .T. ) ;
#8324 = CYLINDRICAL_SURFACE ( 'NONE', #2619, 5.000000000000000888 ) ;
#8326 = CIRCLE ( 'NONE', #12215, 3.000000000000002665 ) ;
#8327 = EDGE_CURVE ( 'NONE', #1613, #12145, #14551, .T. ) ;
#8328 = DIRECTION ( 'NONE',  ( 0.000000000000000000, 0.000000000000000000, 1.000000000000000000 ) ) ;
#8329 = ORIENTED_EDGE ( 'NONE', *, *, #7554, .F. ) ;
#8330 = ORIENTED_EDGE ( 'NONE', *, *, #13396, .T. ) ;
#8331 = LINE ( 'NONE', #7183, #11795 ) ;
#8332 = ORIENTED_EDGE ( 'NONE', *, *, #2945, .T. ) ;
#8333 =( REPRESENTATION_RELATIONSHIP ('NONE','NONE', #12187, #5964 ) REPRESENTATION_RELATIONSHIP_WITH_TRANSFORMATION ( #2365 )SHAPE_REPRESENTATION_RELATIONSHIP( ) );
#8334 = VECTOR ( 'NONE', #10480, 1000.000000000000000 ) ;
#8335 = CARTESIAN_POINT ( 'NONE',  ( 37.53686968382241673, 89.89283556784525331, -10.50000000000000000 ) ) ;
#8336 = ADVANCED_FACE ( 'NONE', ( #1438 ), #7263, .F. ) ;
#8337 = DIRECTION ( 'NONE',  ( -0.000000000000000000, -0.000000000000000000, 1.000000000000000000 ) ) ;
#8338 = CIRCLE ( 'NONE', #11007, 53.55662432702593634 ) ;
#8339 = CARTESIAN_POINT ( 'NONE',  ( 0.000000000000000000, 0.000000000000000000, 0.000000000000000000 ) ) ;
#8340 = DIRECTION ( 'NONE',  ( 1.000000000000000000, 0.000000000000000000, 0.000000000000000000 ) ) ;
#8341 = ORIENTED_EDGE ( 'NONE', *, *, #13933, .T. ) ;
#8342 = DIRECTION ( 'NONE',  ( 1.000000000000000000, 0.000000000000000000, 0.000000000000000000 ) ) ;
#8343 = CYLINDRICAL_SURFACE ( 'NONE', #8712, 0.5000000000000043299 ) ;
#8344 = ORIENTED_EDGE ( 'NONE', *, *, #13441, .T. ) ;
#8345 = CARTESIAN_POINT ( 'NONE',  ( 100.0000000000000000, -3.430248998885766286E-13, 8.000000000000000000 ) ) ;
#8346 = EDGE_CURVE ( 'NONE', #6889, #2988, #522, .T. ) ;
#8347 = ADVANCED_FACE ( 'NONE', ( #3867 ), #4851, .T. ) ;
#8348 = VECTOR ( 'NONE', #13191, 1000.000000000000000 ) ;
#8349 = ORIENTED_EDGE ( 'NONE', *, *, #921, .F. ) ;
#8350 = AXIS2_PLACEMENT_3D ( 'NONE', #14410, #10686, #2489 ) ;
#8351 = ORIENTED_EDGE ( 'NONE', *, *, #1652, .F. ) ;
#8352 = CARTESIAN_POINT ( 'NONE',  ( 3.999999999999995559, -1.942223658245636253, -0.3516579909967626483 ) ) ;
#8353 = CARTESIAN_POINT ( 'NONE',  ( -12.86891638962156215, 56.43380494353993271, 10.49999999999999822 ) ) ;
#8354 = ORIENTED_EDGE ( 'NONE', *, *, #5567, .F. ) ;
#8355 = CARTESIAN_POINT ( 'NONE',  ( 31.59365702568383938, 102.2290646705776282, -12.13969626787233835 ) ) ;
#8356 = AXIS2_PLACEMENT_3D ( 'NONE', #5938, #10352, #2308 ) ;
#8357 = DIRECTION ( 'NONE',  ( -1.000000000000000000, 0.000000000000000000, 0.000000000000000000 ) ) ;
#8358 = FACE_OUTER_BOUND ( 'NONE', #1030, .T. ) ;
#8359 = CARTESIAN_POINT ( 'NONE',  ( 19.68583958711425552, -30.74264578624780597, -28.00000000000000000 ) ) ;
#8360 = AXIS2_PLACEMENT_3D ( 'NONE', #4145, #5571, #11351 ) ;
#8361 = AXIS2_PLACEMENT_3D ( 'NONE', #13361, #10930, #12013 ) ;
#8362 = CARTESIAN_POINT ( 'NONE',  ( 22.33583958711425055, -30.74264578624780597, 14.49999999999999822 ) ) ;
#8363 = ORIENTED_EDGE ( 'NONE', *, *, #7692, .F. ) ;
#8364 = CARTESIAN_POINT ( 'NONE',  ( 20.00000000000000000, 0.000000000000000000, -25.50000000000000355 ) ) ;
#8365 = EDGE_LOOP ( 'NONE', ( #2250, #4078 ) ) ;
#8366 = CARTESIAN_POINT ( 'NONE',  ( -12.18091848848563430, 106.3044177073317087, -16.76518324937863014 ) ) ;
#8367 = CARTESIAN_POINT ( 'NONE',  ( 38.26834323650903968, 92.38795325112864987, -8.000000000000000000 ) ) ;
#8368 = AXIS2_PLACEMENT_3D ( 'NONE', #11951, #241, #6156 ) ;
#8369 = CARTESIAN_POINT ( 'NONE',  ( 57.06275842387049835, -9.706953719245678514, 8.000000000000000000 ) ) ;
#8370 = AXIS2_PLACEMENT_3D ( 'NONE', #12455, #3190, #992 ) ;
#8371 = CARTESIAN_POINT ( 'NONE',  ( -42.50536573064432133, -32.06294366074479996, -10.50000000000000000 ) ) ;
#8372 = VERTEX_POINT ( 'NONE', #6049 ) ;
#8373 = EDGE_CURVE ( 'NONE', #14780, #8393, #2655, .T. ) ;
#8374 = CARTESIAN_POINT ( 'NONE',  ( -42.04772703543551415, -32.26435573746212526, 8.000000000000000000 ) ) ;
#8375 = ORIENTED_EDGE ( 'NONE', *, *, #5136, .F. ) ;
#8376 = ORIENTED_EDGE ( 'NONE', *, *, #2845, .T. ) ;
#8377 = CARTESIAN_POINT ( 'NONE',  ( -23.49999999999971223, -45.89934640057541060, 8.000000000000000000 ) ) ;
#8378 = CYLINDRICAL_SURFACE ( 'NONE', #7807, 59.50000000000000000 ) ;
#8379 = CIRCLE ( 'NONE', #4512, 2.649999999999985700 ) ;
#8380 = CIRCLE ( 'NONE', #6677, 75.00000000000001421 ) ;
#8381 = CARTESIAN_POINT ( 'NONE',  ( -32.10716661655236948, 102.0615849490104949, -13.52016324361725275 ) ) ;
#8382 = DIRECTION ( 'NONE',  ( 0.000000000000000000, 0.000000000000000000, -1.000000000000000000 ) ) ;
#8383 = VERTEX_POINT ( 'NONE', #14196 ) ;
#8384 = PLANE ( 'NONE',  #895 ) ;
#8385 = DIRECTION ( 'NONE',  ( 1.000000000000000000, 0.000000000000000000, 0.000000000000000000 ) ) ;
#8386 = CARTESIAN_POINT ( 'NONE',  ( -36.14014761921588104, 11.74264578624790190, -25.50000000000000355 ) ) ;
#8387 = VECTOR ( 'NONE', #14235, 1000.000000000000000 ) ;
#8388 = EDGE_CURVE ( 'NONE', #2149, #12781, #6765, .T. ) ;
#8389 = VERTEX_POINT ( 'NONE', #4937 ) ;
#8390 = ADVANCED_FACE ( 'NONE', ( #9616 ), #443, .T. ) ;
#8391 = ADVANCED_FACE ( 'NONE', ( #14415 ), #8343, .F. ) ;
#8392 = ORIENTED_EDGE ( 'NONE', *, *, #3225, .F. ) ;
#8393 = VERTEX_POINT ( 'NONE', #6205 ) ;
#8394 = DIRECTION ( 'NONE',  ( 0.000000000000000000, 0.000000000000000000, 1.000000000000000000 ) ) ;
#8395 = FACE_OUTER_BOUND ( 'NONE', #2186, .T. ) ;
#8396 = DIRECTION ( 'NONE',  ( 1.000000000000000000, 0.000000000000000000, 0.000000000000000000 ) ) ;
#8397 = FACE_BOUND ( 'NONE', #1730, .T. ) ;
#8398 = SURFACE_SIDE_STYLE ('',( #3847 ) ) ;
#8399 = CARTESIAN_POINT ( 'NONE',  ( -29.70588235294118107, 96.53269163155674448, -10.99999999999999645 ) ) ;
#8400 = AXIS2_PLACEMENT_3D ( 'NONE', #3122, #6220, #10940 ) ;
#8401 = EDGE_CURVE ( 'NONE', #11699, #604, #8467, .T. ) ;
#8402 = VERTEX_POINT ( 'NONE', #9472 ) ;
#8403 = ORIENTED_EDGE ( 'NONE', *, *, #5268, .T. ) ;
#8404 = VERTEX_POINT ( 'NONE', #11775 ) ;
#8405 = DIRECTION ( 'NONE',  ( 0.000000000000000000, 0.000000000000000000, 1.000000000000000000 ) ) ;
#8406 = CARTESIAN_POINT ( 'NONE',  ( -47.21331623427138879, -33.48561063518577896, -13.00000000000000178 ) ) ;
#8407 = DIRECTION ( 'NONE',  ( -1.000000000000000000, 0.000000000000000000, 0.000000000000000000 ) ) ;
#8408 = ORIENTED_EDGE ( 'NONE', *, *, #4130, .F. ) ;
#8409 = EDGE_LOOP ( 'NONE', ( #9819, #258, #6332, #6035 ) ) ;
#8410 = DIRECTION ( 'NONE',  ( -1.000000000000000000, 0.000000000000000000, 0.000000000000000000 ) ) ;
#8411 = CIRCLE ( 'NONE', #13022, 0.5000000000000004441 ) ;
#8412 = VERTEX_POINT ( 'NONE', #214 ) ;
#8413 = CARTESIAN_POINT ( 'NONE',  ( -68.58935777509427112, 68.58935777509594800, -8.000000000000000000 ) ) ;
#8414 = EDGE_CURVE ( 'NONE', #11296, #5532, #235, .T. ) ;
#8415 = DIRECTION ( 'NONE',  ( 1.000000000000000000, 0.000000000000000000, 0.000000000000000000 ) ) ;
#8416 = LINE ( 'NONE', #7111, #11904 ) ;
#8417 = VERTEX_POINT ( 'NONE', #7192 ) ;
#8418 = DIRECTION ( 'NONE',  ( 0.000000000000000000, 0.000000000000000000, -1.000000000000000000 ) ) ;
#8419 = CARTESIAN_POINT ( 'NONE',  ( 68.58935777509475429, -68.58935777509547904, -10.50000000000000000 ) ) ;
#8420 = EDGE_CURVE ( 'NONE', #12827, #7196, #10411, .T. ) ;
#8421 = VERTEX_POINT ( 'NONE', #12905 ) ;
#8422 = DIRECTION ( 'NONE',  ( -1.000000000000000000, 0.000000000000000000, 0.000000000000000000 ) ) ;
#8423 = VERTEX_POINT ( 'NONE', #10618 ) ;
#8424 = ORIENTED_EDGE ( 'NONE', *, *, #12801, .T. ) ;
#8425 = CARTESIAN_POINT ( 'NONE',  ( -24.98583958711379083, -30.74264578624812927, -25.50000000000000355 ) ) ;
#8426 = DIRECTION ( 'NONE',  ( -1.000000000000000000, 0.000000000000000000, 0.000000000000000000 ) ) ;
#8427 = EDGE_CURVE ( 'NONE', #9614, #3630, #5798, .T. ) ;
#8428 = AXIS2_PLACEMENT_3D ( 'NONE', #5677, #13809, #6362 ) ;
#8429 = EDGE_CURVE ( 'NONE', #469, #14514, #2947, .T. ) ;
#8430 = DIRECTION ( 'NONE',  ( -1.000000000000000000, 0.000000000000000000, 0.000000000000000000 ) ) ;
#8431 = CYLINDRICAL_SURFACE ( 'NONE', #8735, 0.5000000000000004441 ) ;
#8432 = DIRECTION ( 'NONE',  ( 1.000000000000000000, 0.000000000000000000, 0.000000000000000000 ) ) ;
#8433 = DIRECTION ( 'NONE',  ( -1.000000000000000000, 0.000000000000000000, 0.000000000000000000 ) ) ;
#8434 = ORIENTED_EDGE ( 'NONE', *, *, #14365, .F. ) ;
#8435 = CARTESIAN_POINT ( 'NONE',  ( 0.000000000000000000, 0.000000000000000000, 8.000000000000000000 ) ) ;
#8436 = ORIENTED_EDGE ( 'NONE', *, *, #14810, .T. ) ;
#8437 = EDGE_CURVE ( 'NONE', #7919, #9694, #7540, .T. ) ;
#8438 = CARTESIAN_POINT ( 'NONE',  ( -52.54657765281192638, 6.917888187662934563, -8.000000000000000000 ) ) ;
#8439 = CARTESIAN_POINT ( 'NONE',  ( -7.500000000000000000, 74.62405778299650194, -20.00000000000000000 ) ) ;
#8440 = DIRECTION ( 'NONE',  ( -1.000000000000000000, 0.000000000000000000, 0.000000000000000000 ) ) ;
#8441 = DIRECTION ( 'NONE',  ( -0.000000000000000000, -0.000000000000000000, 1.000000000000000000 ) ) ;
#8442 = ORIENTED_EDGE ( 'NONE', *, *, #1608, .T. ) ;
#8443 = EDGE_LOOP ( 'NONE', ( #4464, #7833, #13814, #8344 ) ) ;
#8444 = DIRECTION ( 'NONE',  ( -1.000000000000000000, 0.000000000000000000, 0.000000000000000000 ) ) ;
#8445 = ORIENTED_EDGE ( 'NONE', *, *, #10347, .T. ) ;
#8446 = EDGE_CURVE ( 'NONE', #13092, #11131, #11447, .T. ) ;
#8447 = DIRECTION ( 'NONE',  ( 1.000000000000000000, 0.000000000000000000, 0.000000000000000000 ) ) ;
#8448 = CARTESIAN_POINT ( 'NONE',  ( 57.06275842387049835, -9.706953719245678514, -13.00000000000000178 ) ) ;
#8449 = DIRECTION ( 'NONE',  ( 1.000000000000000000, -7.105427357601001859E-15, 0.000000000000000000 ) ) ;
#8450 = CARTESIAN_POINT ( 'NONE',  ( 27.00670028307162340, 46.24878538001323136, -10.50000000000000000 ) ) ;
#8451 = ORIENTED_EDGE ( 'NONE', *, *, #10092, .F. ) ;
#8452 = CARTESIAN_POINT ( 'NONE',  ( 6.917888187663118416, 52.54657765281190507, 10.49999999999999822 ) ) ;
#8453 = CARTESIAN_POINT ( 'NONE',  ( -51.19406879332065330, -13.71740939043347041, -10.50000000000000000 ) ) ;
#8454 = CARTESIAN_POINT ( 'NONE',  ( 49.00442420935993226, -30.80502811811213704, -10.50000000000000000 ) ) ;
#8455 = ORIENTED_EDGE ( 'NONE', *, *, #3255, .F. ) ;
#8456 = CARTESIAN_POINT ( 'NONE',  ( 47.21331623427115431, 33.48561063518610581, -13.00000000000000178 ) ) ;
#8457 = AXIS2_PLACEMENT_3D ( 'NONE', #8966, #13604, #13688 ) ;
#8458 = ORIENTED_EDGE ( 'NONE', *, *, #12206, .F. ) ;
#8459 = CARTESIAN_POINT ( 'NONE',  ( 36.52608637591580987, -92.55687898036916295, -8.000000000000000000 ) ) ;
#8460 = DIRECTION ( 'NONE',  ( 0.000000000000000000, 0.000000000000000000, 1.000000000000000000 ) ) ;
#8461 = FACE_BOUND ( 'NONE', #6441, .T. ) ;
#8462 = CARTESIAN_POINT ( 'NONE',  ( -32.07879498588596334, 95.77069236132481933, -15.33800373393474281 ) ) ;
#8463 = EDGE_CURVE ( 'NONE', #3549, #7242, #9480, .T. ) ;
#8464 = VERTEX_POINT ( 'NONE', #9922 ) ;
#8465 = ADVANCED_FACE ( 'NONE', ( #7653 ), #12442, .F. ) ;
#8466 = DIRECTION ( 'NONE',  ( 0.000000000000000000, 0.000000000000000000, -1.000000000000000000 ) ) ;
#8467 = CIRCLE ( 'NONE', #1923, 14.00000000000000000 ) ;
#8469 = EDGE_CURVE ( 'NONE', #13798, #5235, #13373, .T. ) ;
#8468 = CARTESIAN_POINT ( 'NONE',  ( -32.26435573746199736, 42.04772703543562073, -8.000000000000000000 ) ) ;
#8470 = DIRECTION ( 'NONE',  ( 1.000000000000000000, 0.000000000000000000, 0.000000000000000000 ) ) ;
#8471 = VERTEX_POINT ( 'NONE', #14572 ) ;
#8472 = ORIENTED_EDGE ( 'NONE', *, *, #817, .F. ) ;
#8473 = CARTESIAN_POINT ( 'NONE',  ( -18.52941176470586981, 60.21346111671361001, 26.00000000000000000 ) ) ;
#8474 = EDGE_CURVE ( 'NONE', #4578, #2618, #9241, .T. ) ;
#8475 = DIRECTION ( 'NONE',  ( -1.000000000000000000, 0.000000000000000000, 0.000000000000000000 ) ) ;
#8476 = ORIENTED_EDGE ( 'NONE', *, *, #11876, .F. ) ;
#8477 = CIRCLE ( 'NONE', #7985, 56.99999999999999289 ) ;
#8478 = DIRECTION ( 'NONE',  ( 0.000000000000000000, 0.000000000000000000, -1.000000000000000000 ) ) ;
#8479 = DIRECTION ( 'NONE',  ( 0.000000000000000000, 0.000000000000000000, -1.000000000000000000 ) ) ;
#8480 = CYLINDRICAL_SURFACE ( 'NONE', #12381, 59.50000000000000000 ) ;
#8481 = ORIENTED_EDGE ( 'NONE', *, *, #6088, .F. ) ;
#8482 = PLANE ( 'NONE',  #8995 ) ;
#8483 = CARTESIAN_POINT ( 'NONE',  ( -12.50000000000000000, 40.62019202317981126, -23.50000000000000000 ) ) ;
#8484 = ORIENTED_EDGE ( 'NONE', *, *, #8522, .T. ) ;
#8485 = EDGE_CURVE ( 'NONE', #9901, #6334, #13131, .T. ) ;
#8486 = CARTESIAN_POINT ( 'NONE',  ( 0.000000000000000000, 0.000000000000000000, -10.50000000000000000 ) ) ;
#8487 = AXIS2_PLACEMENT_3D ( 'NONE', #11337, #12392, #4281 ) ;
#8488 = VERTEX_POINT ( 'NONE', #4176 ) ;
#8489 = AXIS2_PLACEMENT_3D ( 'NONE', #13840, #14906, #7053 ) ;
#8490 = AXIS2_PLACEMENT_3D ( 'NONE', #9326, #13978, #3571 ) ;
#8491 = ORIENTED_EDGE ( 'NONE', *, *, #2677, .F. ) ;
#8492 = DIRECTION ( 'NONE',  ( 1.000000000000000000, 0.000000000000000000, 0.000000000000000000 ) ) ;
#8493 = CARTESIAN_POINT ( 'NONE',  ( -52.36539807335606156, 6.451868917687758831, -10.50000000000000000 ) ) ;
#8494 = DIRECTION ( 'NONE',  ( -1.000000000000000000, 0.000000000000000000, 0.000000000000000000 ) ) ;
#8495 = STYLED_ITEM ( 'NONE', ( #3643 ), #9343 ) ;
#8496 = AXIS2_PLACEMENT_3D ( 'NONE', #5306, #7662, #6583 ) ;
#8497 = LINE ( 'NONE', #10855, #1818 ) ;
#8498 = CARTESIAN_POINT ( 'NONE',  ( -31.76435573746199381, 42.04772703543562073, -13.00000000000000178 ) ) ;
#8499 = CARTESIAN_POINT ( 'NONE',  ( -37.12029293941250074, 89.61631465359532456, 10.49999999999999822 ) ) ;
#8500 = AXIS2_PLACEMENT_3D ( 'NONE', #11979, #13106, #2703 ) ;
#8501 = DIRECTION ( 'NONE',  ( 0.000000000000000000, 0.000000000000000000, 1.000000000000000000 ) ) ;
#8502 = CIRCLE ( 'NONE', #22, 22.00000000000001421 ) ;
#8503 = ORIENTED_EDGE ( 'NONE', *, *, #2354, .F. ) ;
#8504 = DIRECTION ( 'NONE',  ( -0.000000000000000000, -0.000000000000000000, 1.000000000000000000 ) ) ;
#8505 = ORIENTED_EDGE ( 'NONE', *, *, #12371, .F. ) ;
#8506 = CARTESIAN_POINT ( 'NONE',  ( -11.99241863490640903, 106.3259041464359882, -17.21938144708833462 ) ) ;
#8507 = DIRECTION ( 'NONE',  ( -0.000000000000000000, -0.000000000000000000, 1.000000000000000000 ) ) ;
#8508 = EDGE_CURVE ( 'NONE', #9888, #5327, #6813, .T. ) ;
#8509 = AXIS2_PLACEMENT_3D ( 'NONE', #13347, #11230, #8787 ) ;
#8510 = EDGE_CURVE ( 'NONE', #1401, #4053, #10692, .T. ) ;
#8511 = CARTESIAN_POINT ( 'NONE',  ( 0.000000000000000000, 0.000000000000000000, -10.50000000000000000 ) ) ;
#8512 = CIRCLE ( 'NONE', #5845, 3.000000000000002665 ) ;
#8513 = FACE_OUTER_BOUND ( 'NONE', #11215, .T. ) ;
#8514 = EDGE_CURVE ( 'NONE', #11572, #14934, #6942, .T. ) ;
#8515 = VECTOR ( 'NONE', #10198, 1000.000000000000114 ) ;
#8516 = ORIENTED_EDGE ( 'NONE', *, *, #7968, .T. ) ;
#8517 = DIRECTION ( 'NONE',  ( 1.000000000000000000, 0.000000000000000000, 0.000000000000000000 ) ) ;
#8518 = EDGE_LOOP ( 'NONE', ( #2081, #290, #9862, #7894 ) ) ;
#8519 = ORIENTED_EDGE ( 'NONE', *, *, #532, .F. ) ;
#8520 = FACE_OUTER_BOUND ( 'NONE', #2604, .T. ) ;
#8521 = CARTESIAN_POINT ( 'NONE',  ( 56.43380494353997534, 12.86891638962136319, 10.49999999999999822 ) ) ;
#8522 = EDGE_CURVE ( 'NONE', #7016, #11742, #4161, .T. ) ;
#8523 = VECTOR ( 'NONE', #9194, 1000.000000000000114 ) ;
#8524 = DIRECTION ( 'NONE',  ( 0.000000000000000000, 0.000000000000000000, -1.000000000000000000 ) ) ;
#8525 = DIRECTION ( 'NONE',  ( -0.000000000000000000, -0.000000000000000000, 1.000000000000000000 ) ) ;
#8526 = DIRECTION ( 'NONE',  ( 0.000000000000000000, 0.000000000000000000, 1.000000000000000000 ) ) ;
#8527 = ORIENTED_EDGE ( 'NONE', *, *, #12574, .F. ) ;
#8528 = AXIS2_PLACEMENT_3D ( 'NONE', #7465, #8337, #208 ) ;
#8529 = DIRECTION ( 'NONE',  ( 1.000000000000000000, 0.000000000000000000, 0.000000000000000000 ) ) ;
#8530 = LINE ( 'NONE', #13173, #9797 ) ;
#8531 = EDGE_CURVE ( 'NONE', #10105, #1597, #12360, .T. ) ;
#8532 = CARTESIAN_POINT ( 'NONE',  ( -13.71740939043329277, 51.19406879332069593, -10.50000000000000000 ) ) ;
#8533 = EDGE_LOOP ( 'NONE', ( #5142, #10683, #2356, #13427 ) ) ;
#8534 = CYLINDRICAL_SURFACE ( 'NONE', #3423, 2.649999999999985700 ) ;
#8535 = ORIENTED_EDGE ( 'NONE', *, *, #6372, .F. ) ;
#8536 = CARTESIAN_POINT ( 'NONE',  ( 3.999999999999996447, 2.309401076758498039, -5.000000000000000888 ) ) ;
#8537 = VERTEX_POINT ( 'NONE', #6652 ) ;
#8538 = CARTESIAN_POINT ( 'NONE',  ( 9.442781676091986043, 62.28890912541182701, -19.61600713740890356 ) ) ;
#8539 = CARTESIAN_POINT ( 'NONE',  ( 0.000000000000000000, 0.000000000000000000, -8.000000000000000000 ) ) ;
#8540 = CARTESIAN_POINT ( 'NONE',  ( 89.61631465359491244, 37.12029293941346708, -13.00000000000000178 ) ) ;
#8541 = ORIENTED_EDGE ( 'NONE', *, *, #7548, .T. ) ;
#8542 = VECTOR ( 'NONE', #7390, 1000.000000000000000 ) ;
#8543 = LINE ( 'NONE', #4921, #8348 ) ;
#8544 = CARTESIAN_POINT ( 'NONE',  ( 7.500000000000000888, 106.7368258849775202, -20.00000000000000000 ) ) ;
#8545 = VECTOR ( 'NONE', #12776, 1000.000000000000000 ) ;
#8546 = DIRECTION ( 'NONE',  ( 0.000000000000000000, 0.000000000000000000, 1.000000000000000000 ) ) ;
#8547 = ORIENTED_EDGE ( 'NONE', *, *, #9029, .T. ) ;
#8548 = CIRCLE ( 'NONE', #4945, 53.55662432702593634 ) ;
#8549 = ORIENTED_EDGE ( 'NONE', *, *, #13626, .F. ) ;
#8550 = DIRECTION ( 'NONE',  ( 0.000000000000000000, 0.000000000000000000, 1.000000000000000000 ) ) ;
#8551 = VERTEX_POINT ( 'NONE', #10148 ) ;
#8552 = EDGE_CURVE ( 'NONE', #11984, #6973, #4020, .T. ) ;
#8553 = DIRECTION ( 'NONE',  ( 0.000000000000000000, 0.000000000000000000, -1.000000000000000000 ) ) ;
#8554 = DIRECTION ( 'NONE',  ( -1.000000000000000000, 0.000000000000000000, 0.000000000000000000 ) ) ;
#8555 =( NAMED_UNIT ( * ) PLANE_ANGLE_UNIT ( ) SI_UNIT ( $, .RADIAN. ) );
#8556 = AXIS2_PLACEMENT_3D ( 'NONE', #13166, #1472, #2761 ) ;
#8557 = FACE_OUTER_BOUND ( 'NONE', #11384, .T. ) ;
#8558 = CARTESIAN_POINT ( 'NONE',  ( 2.449293598294700991E-16, -97.00000000000000000, -13.00000000000000178 ) ) ;
#8559 = ORIENTED_EDGE ( 'NONE', *, *, #10369, .F. ) ;
#8560 = PLANE ( 'NONE',  #4883 ) ;
#8561 = CIRCLE ( 'NONE', #7586, 60.50000000000000000 ) ;
#8562 = VERTEX_POINT ( 'NONE', #1738 ) ;
#8563 = EDGE_LOOP ( 'NONE', ( #12211, #4054 ) ) ;
#8564 = CARTESIAN_POINT ( 'NONE',  ( 0.000000000000000000, -4.862606272033110244, -3.745885042887441063 ) ) ;
#8565 = CIRCLE ( 'NONE', #1786, 0.5000000000000073275 ) ;
#8566 = EDGE_CURVE ( 'NONE', #198, #11105, #5368, .T. ) ;
#8567 = EDGE_CURVE ( 'NONE', #13490, #12729, #9966, .T. ) ;
#8568 = DIRECTION ( 'NONE',  ( 0.000000000000000000, 0.000000000000000000, -1.000000000000000000 ) ) ;
#8569 = DIRECTION ( 'NONE',  ( 1.000000000000000000, 0.000000000000000000, 0.000000000000000000 ) ) ;
#8570 = LINE ( 'NONE', #8498, #11900 ) ;
#8571 = DIRECTION ( 'NONE',  ( -0.000000000000000000, -0.000000000000000000, -1.000000000000000000 ) ) ;
#8572 = CARTESIAN_POINT ( 'NONE',  ( -38.79014761921587962, 11.74264578624790190, -28.00000000000000000 ) ) ;
#8573 = ORIENTED_EDGE ( 'NONE', *, *, #8195, .F. ) ;
#8574 = CIRCLE ( 'NONE', #9537, 10.00000000000000355 ) ;
#8575 = AXIS2_PLACEMENT_3D ( 'NONE', #596, #8479, #11921 ) ;
#8576 = CARTESIAN_POINT ( 'NONE',  ( 27.94117647058824616, 90.79807628710781842, -23.50000000000000000 ) ) ;
#8577 = AXIS2_PLACEMENT_3D ( 'NONE', #14831, #4434, #13689 ) ;
#8578 = ORIENTED_EDGE ( 'NONE', *, *, #4179, .F. ) ;
#8579 = LINE ( 'NONE', #14671, #7678 ) ;
#8580 = DIRECTION ( 'NONE',  ( 1.000000000000000000, -1.778456000581264310E-15, 0.000000000000000000 ) ) ;
#8581 = EDGE_LOOP ( 'NONE', ( #9840, #2917, #11066, #7587, #8224 ) ) ;
#8582 = CARTESIAN_POINT ( 'NONE',  ( 30.68753049492184815, 96.22530292649337014, -14.05553407057507087 ) ) ;
#8583 = ORIENTED_EDGE ( 'NONE', *, *, #817, .T. ) ;
#8584 = AXIS2_PLACEMENT_3D ( 'NONE', #10574, #9201, #1172 ) ;
#8585 = CARTESIAN_POINT ( 'NONE',  ( -3.999999999999996447, -2.309401076758511806, -5.000000000000000888 ) ) ;
#8586 = ORIENTED_EDGE ( 'NONE', *, *, #3367, .T. ) ;
#8587 = AXIS2_PLACEMENT_3D ( 'NONE', #9382, #6954, #14030 ) ;
#8588 = DIRECTION ( 'NONE',  ( 0.000000000000000000, 0.000000000000000000, 1.000000000000000000 ) ) ;
#8589 = VERTEX_POINT ( 'NONE', #9087 ) ;
#8590 = FACE_OUTER_BOUND ( 'NONE', #1726, .T. ) ;
#8591 = CARTESIAN_POINT ( 'NONE',  ( 25.00000000000000000, 81.24038404635960831, -23.50000000000000000 ) ) ;
#8592 = DIRECTION ( 'NONE',  ( 0.000000000000000000, 0.000000000000000000, 1.000000000000000000 ) ) ;
#8593 = EDGE_CURVE ( 'NONE', #9550, #8921, #286, .T. ) ;
#8594 = DIRECTION ( 'NONE',  ( 0.000000000000000000, 0.000000000000000000, -1.000000000000000000 ) ) ;
#8595 = FACE_OUTER_BOUND ( 'NONE', #11446, .T. ) ;
#8596 = AXIS2_PLACEMENT_3D ( 'NONE', #10334, #14974, #4568 ) ;
#8597 = EDGE_CURVE ( 'NONE', #14537, #13133, #14336, .T. ) ;
#8598 = ORIENTED_EDGE ( 'NONE', *, *, #11310, .F. ) ;
#8599 = CIRCLE ( 'NONE', #4255, 44.89637028918153305 ) ;
#8600 = DIRECTION ( 'NONE',  ( 1.000000000000000000, 0.000000000000000000, -0.000000000000000000 ) ) ;
#8601 = DIRECTION ( 'NONE',  ( -0.000000000000000000, -0.000000000000000000, 1.000000000000000000 ) ) ;
#8602 = CIRCLE ( 'NONE', #5937, 0.5000000000000004441 ) ;
#8603 = CARTESIAN_POINT ( 'NONE',  ( 0.000000000000000000, 0.000000000000000000, -10.50000000000000000 ) ) ;
#8604 = EDGE_CURVE ( 'NONE', #10117, #10604, #6316, .T. ) ;
#8605 = ORIENTED_EDGE ( 'NONE', *, *, #5903, .F. ) ;
#8606 = DIRECTION ( 'NONE',  ( 0.000000000000000000, 0.000000000000000000, 1.000000000000000000 ) ) ;
#8607 = CIRCLE ( 'NONE', #6666, 0.5000000000000022204 ) ;
#8608 = ORIENTED_EDGE ( 'NONE', *, *, #6673, .T. ) ;
#8609 = DIRECTION ( 'NONE',  ( 0.000000000000000000, 0.000000000000000000, 1.000000000000000000 ) ) ;
#8610 = CYLINDRICAL_SURFACE ( 'NONE', #3205, 60.50000000000000000 ) ;
#8611 = AXIS2_PLACEMENT_3D ( 'NONE', #7663, #3114, #5308 ) ;
#8612 = ADVANCED_FACE ( 'NONE', ( #14950 ), #974, .F. ) ;
#8613 = DIRECTION ( 'NONE',  ( -0.000000000000000000, -0.000000000000000000, 1.000000000000000000 ) ) ;
#8614 = EDGE_CURVE ( 'NONE', #11081, #6408, #7789, .T. ) ;
#8615 = DIRECTION ( 'NONE',  ( -0.000000000000000000, -0.000000000000000000, 1.000000000000000000 ) ) ;
#8616 = PRODUCT_CONTEXT ( 'NONE', #12313, 'mechanical' ) ;
#8617 = CARTESIAN_POINT ( 'NONE',  ( -29.86558579037015448, 96.48341332593351183, -12.29240575635728838 ) ) ;
#8618 = ORIENTED_EDGE ( 'NONE', *, *, #11746, .T. ) ;
#8619 = ORIENTED_EDGE ( 'NONE', *, *, #844, .F. ) ;
#8620 = CIRCLE ( 'NONE', #13734, 0.5000000000000004441 ) ;
#8621 = CARTESIAN_POINT ( 'NONE',  ( -26.49999999999971578, -45.89934640057541060, -13.00000000000000178 ) ) ;
#8622 = CARTESIAN_POINT ( 'NONE',  ( 0.000000000000000000, 0.000000000000000000, -16.00000000000000000 ) ) ;
#8623 = CARTESIAN_POINT ( 'NONE',  ( -3.999999999999996447, -2.309401076758518911, -0.5000000000000004441 ) ) ;
#8624 = ORIENTED_EDGE ( 'NONE', *, *, #4087, .T. ) ;
#8625 = EDGE_CURVE ( 'NONE', #7688, #10743, #4645, .T. ) ;
#8626 = EDGE_LOOP ( 'NONE', ( #9400, #9863, #6580, #11628, #5065 ) ) ;
#8627 = CARTESIAN_POINT ( 'NONE',  ( -45.46633369868291652, 26.25000000000019895, -10.50000000000000000 ) ) ;
#8628 = VERTEX_POINT ( 'NONE', #7017 ) ;
#8629 = VECTOR ( 'NONE', #797, 1000.000000000000000 ) ;
#8630 = FACE_OUTER_BOUND ( 'NONE', #9179, .T. ) ;
#8631 = FACE_OUTER_BOUND ( 'NONE', #14308, .T. ) ;
#8632 = ORIENTED_EDGE ( 'NONE', *, *, #11770, .T. ) ;
#8633 = ORIENTED_EDGE ( 'NONE', *, *, #5049, .T. ) ;
#8634 = CARTESIAN_POINT ( 'NONE',  ( 7.500000000000007105, 85.00000000000000000, 46.00000000000000000 ) ) ;
#8635 = DIRECTION ( 'NONE',  ( 1.000000000000000000, 0.000000000000000000, 0.000000000000000000 ) ) ;
#8636 = ORIENTED_EDGE ( 'NONE', *, *, #3072, .T. ) ;
#8637 = CARTESIAN_POINT ( 'NONE',  ( -31.74999999999995737, 3.061616997868383634E-16, -2.500000000000028422 ) ) ;
#8638 = CIRCLE ( 'NONE', #7667, 59.50000000000000000 ) ;
#8639 = ORIENTED_EDGE ( 'NONE', *, *, #792, .T. ) ;
#8640 = ORIENTED_EDGE ( 'NONE', *, *, #8346, .T. ) ;
#8641 = DIRECTION ( 'NONE',  ( 1.000000000000000000, 0.000000000000000000, 0.000000000000000000 ) ) ;
#8642 = EDGE_LOOP ( 'NONE', ( #3992, #7659 ) ) ;
#8643 = CARTESIAN_POINT ( 'NONE',  ( 35.50612649840986990, 100.5723974928649511, -15.96895346309147534 ) ) ;
#8644 = CARTESIAN_POINT ( 'NONE',  ( -31.47058823529412663, 102.2673069760056421, -31.00000000000000000 ) ) ;
#8645 = FACE_OUTER_BOUND ( 'NONE', #5071, .T. ) ;
#8646 = DIRECTION ( 'NONE',  ( -1.000000000000000000, 0.000000000000000000, 0.000000000000000000 ) ) ;
#8647 = CARTESIAN_POINT ( 'NONE',  ( -89.61631465359441506, 37.12029293941468211, 8.000000000000000000 ) ) ;
#8648 = ORIENTED_EDGE ( 'NONE', *, *, #10614, .T. ) ;
#8649 = EDGE_CURVE ( 'NONE', #1696, #9753, #3189, .T. ) ;
#8650 = LINE ( 'NONE', #14507, #9227 ) ;
#8651 = LINE ( 'NONE', #2886, #5290 ) ;
#8652 = EDGE_CURVE ( 'NONE', #5062, #8404, #11461, .T. ) ;
#8653 = ADVANCED_FACE ( 'NONE', ( #6796 ), #6722, .T. ) ;
#8654 = ADVANCED_FACE ( 'NONE', ( #13886 ), #8098, .T. ) ;
#8655 = DIRECTION ( 'NONE',  ( 0.000000000000000000, 0.000000000000000000, 1.000000000000000000 ) ) ;
#8656 = FACE_OUTER_BOUND ( 'NONE', #982, .T. ) ;
#8657 = EDGE_LOOP ( 'NONE', ( #11974, #10212 ) ) ;
#8658 = CARTESIAN_POINT ( 'NONE',  ( 31.32379180359345838, 96.02017129613331292, -14.76790389961145245 ) ) ;
#8659 = ORIENTED_EDGE ( 'NONE', *, *, #8927, .T. ) ;
#8660 = CARTESIAN_POINT ( 'NONE',  ( 0.000000000000000000, 0.000000000000000000, -25.50000000000000355 ) ) ;
#8661 = ORIENTED_EDGE ( 'NONE', *, *, #12606, .F. ) ;
#8662 = LINE ( 'NONE', #2680, #11885 ) ;
#8663 = VERTEX_POINT ( 'NONE', #4690 ) ;
#8664 = VERTEX_POINT ( 'NONE', #12585 ) ;
#8665 = CARTESIAN_POINT ( 'NONE',  ( 11.99241863490641080, 106.3259041464360024, 17.21938144708833462 ) ) ;
#8666 = CARTESIAN_POINT ( 'NONE',  ( -42.89934640057513349, 26.50000000000019540, -8.000000000000000000 ) ) ;
#8667 = DIRECTION ( 'NONE',  ( -0.000000000000000000, -0.000000000000000000, -1.000000000000000000 ) ) ;
#8668 = CARTESIAN_POINT ( 'NONE',  ( -52.50000000000000711, 0.000000000000000000, -10.50000000000000000 ) ) ;
#8669 = LINE ( 'NONE', #558, #1801 ) ;
#8670 = CARTESIAN_POINT ( 'NONE',  ( -45.89934640057513349, 26.50000000000019540, -10.50000000000000000 ) ) ;
#8671 = CIRCLE ( 'NONE', #9396, 0.5000000000000004441 ) ;
#8672 = ORIENTED_EDGE ( 'NONE', *, *, #7474, .T. ) ;
#8673 = EDGE_CURVE ( 'NONE', #9159, #6576, #13608, .T. ) ;
#8674 = CARTESIAN_POINT ( 'NONE',  ( 9.917888187663120192, 52.54657765281190507, -8.000000000000000000 ) ) ;
#8675 = CARTESIAN_POINT ( 'NONE',  ( 96.58511096861892042, 0.2790467552928839190, -13.00000000000000178 ) ) ;
#8676 = UNCERTAINTY_MEASURE_WITH_UNIT (LENGTH_MEASURE( 1.000000000000000082E-05 ), #6419, 'distance_accuracy_value', 'NONE');
#8677 = CARTESIAN_POINT ( 'NONE',  ( -57.06275842387042729, 9.706953719246069312, 8.000000000000000000 ) ) ;
#8678 = EDGE_LOOP ( 'NONE', ( #1655, #6953, #7696, #14175 ) ) ;
#8679 = CARTESIAN_POINT ( 'NONE',  ( -3.472371940586000072, -2.614027278893185979, -3.320322319202478223 ) ) ;
#8680 = VERTEX_POINT ( 'NONE', #8173 ) ;
#8681 = DIRECTION ( 'NONE',  ( 1.000000000000000000, 0.000000000000000000, 0.000000000000000000 ) ) ;
#8682 = CARTESIAN_POINT ( 'NONE',  ( -52.04657765281192638, 6.917888187662934563, -13.00000000000000178 ) ) ;
#8683 = DIRECTION ( 'NONE',  ( -0.000000000000000000, 0.000000000000000000, 1.000000000000000000 ) ) ;
#8684 = CARTESIAN_POINT ( 'NONE',  ( 47.21331623427115431, 33.48561063518610581, 8.000000000000000000 ) ) ;
#8685 = CARTESIAN_POINT ( 'NONE',  ( -5.510910596163088569E-16, 38.00000000000000000, -33.00000000000000000 ) ) ;
#8686 = ORIENTED_EDGE ( 'NONE', *, *, #4264, .F. ) ;
#8687 = VERTEX_POINT ( 'NONE', #1056 ) ;
#8688 = DIRECTION ( 'NONE',  ( -0.000000000000000000, -0.000000000000000000, 1.000000000000000000 ) ) ;
#8689 = DIRECTION ( 'NONE',  ( 0.000000000000000000, 0.000000000000000000, -1.000000000000000000 ) ) ;
#8690 = CARTESIAN_POINT ( 'NONE',  ( -12.86891638962156215, 56.43380494353993271, -8.000000000000000000 ) ) ;
#8691 = ORIENTED_EDGE ( 'NONE', *, *, #6748, .F. ) ;
#8692 = EDGE_CURVE ( 'NONE', #2935, #14, #521, .T. ) ;
#8693 = ADVANCED_FACE ( 'NONE', ( #5674 ), #9160, .F. ) ;
#8694 = ORIENTED_EDGE ( 'NONE', *, *, #3523, .T. ) ;
#8695 = ORIENTED_EDGE ( 'NONE', *, *, #2351, .F. ) ;
#8696 = EDGE_CURVE ( 'NONE', #3819, #3199, #12639, .T. ) ;
#8697 = CARTESIAN_POINT ( 'NONE',  ( -18.52941176470586981, 60.21346111671361001, -31.00000000000000000 ) ) ;
#8698 = CARTESIAN_POINT ( 'NONE',  ( 0.000000000000000000, -4.862606272033110244, -3.745885042887441063 ) ) ;
#8699 = EDGE_CURVE ( 'NONE', #10230, #11793, #12770, .T. ) ;
#8700 = AXIS2_PLACEMENT_3D ( 'NONE', #9271, #4511, #1307 ) ;
#8701 = ORIENTED_EDGE ( 'NONE', *, *, #11727, .T. ) ;
#8702 = DIRECTION ( 'NONE',  ( 0.000000000000000000, 0.000000000000000000, 1.000000000000000000 ) ) ;
#8703 = DIRECTION ( 'NONE',  ( 0.000000000000000000, 0.000000000000000000, -1.000000000000000000 ) ) ;
#8704 = VERTEX_POINT ( 'NONE', #11681 ) ;
#8705 = LINE ( 'NONE', #5386, #11407 ) ;
#8706 = ORIENTED_EDGE ( 'NONE', *, *, #12561, .T. ) ;
#8707 =( GEOMETRIC_REPRESENTATION_CONTEXT ( 3 ) GLOBAL_UNCERTAINTY_ASSIGNED_CONTEXT ( ( #3987 ) ) GLOBAL_UNIT_ASSIGNED_CONTEXT ( ( #13732, #11455, #7869 ) ) REPRESENTATION_CONTEXT ( 'NONE', 'WORKASPACE' ) );
#8708 = AXIS2_PLACEMENT_3D ( 'NONE', #13378, #2066, #10176 ) ;
#8709 = EDGE_CURVE ( 'NONE', #5953, #11449, #2454, .T. ) ;
#8710 = VERTEX_POINT ( 'NONE', #4060 ) ;
#8711 = DIRECTION ( 'NONE',  ( -1.000000000000000000, 0.000000000000000000, 0.000000000000000000 ) ) ;
#8712 = AXIS2_PLACEMENT_3D ( 'NONE', #8558, #10771, #13055 ) ;
#8713 = AXIS2_PLACEMENT_3D ( 'NONE', #313, #8571, #14213 ) ;
#8714 = CYLINDRICAL_SURFACE ( 'NONE', #270, 3.000000000000002665 ) ;
#8715 = DIRECTION ( 'NONE',  ( -1.000000000000000000, 0.000000000000000000, 0.000000000000000000 ) ) ;
#8716 = FACE_OUTER_BOUND ( 'NONE', #14368, .T. ) ;
#8717 = CARTESIAN_POINT ( 'NONE',  ( 29.51438936481373077, 47.21331623427104063, 8.000000000000000000 ) ) ;
#8718 = AXIS2_PLACEMENT_3D ( 'NONE', #9628, #11854, #10852 ) ;
#8719 = DIRECTION ( 'NONE',  ( 0.000000000000000000, 0.000000000000000000, 1.000000000000000000 ) ) ;
#8720 = ORIENTED_EDGE ( 'NONE', *, *, #5240, .T. ) ;
#8721 = AXIS2_PLACEMENT_3D ( 'NONE', #4122, #11186, #12173 ) ;
#8722 = CARTESIAN_POINT ( 'NONE',  ( -68.58935777509570642, -68.58935777509452691, -13.00000000000000178 ) ) ;
#8723 = CYLINDRICAL_SURFACE ( 'NONE', #13045, 56.99999999999999289 ) ;
#8724 = CIRCLE ( 'NONE', #8490, 50.00000000000000000 ) ;
#8725 = DIRECTION ( 'NONE',  ( 1.000000000000000000, 0.000000000000000000, 0.000000000000000000 ) ) ;
#8726 = CARTESIAN_POINT ( 'NONE',  ( 0.000000000000000000, -4.862606272033110244, -3.745885042887441063 ) ) ;
#8727 = ORIENTED_EDGE ( 'NONE', *, *, #14004, .F. ) ;
#8728 = CARTESIAN_POINT ( 'NONE',  ( 34.13789339514568155, 95.05636893381512209, -16.00000000000000355 ) ) ;
#8729 = VECTOR ( 'NONE', #14217, 1000.000000000000114 ) ;
#8730 = ORIENTED_EDGE ( 'NONE', *, *, #12705, .T. ) ;
#8731 = TOROIDAL_SURFACE ( 'NONE', #6786, 2.700000000000000622, 0.2000000000000000111 ) ;
#8732 = PLANE ( 'NONE',  #6633 ) ;
#8733 = VERTEX_POINT ( 'NONE', #1849 ) ;
#8734 = CARTESIAN_POINT ( 'NONE',  ( -41.65105036528990468, -31.95997502295777792, -10.50000000000000000 ) ) ;
#8735 = AXIS2_PLACEMENT_3D ( 'NONE', #2739, #14057, #11941 ) ;
#8736 = ORIENTED_EDGE ( 'NONE', *, *, #9810, .F. ) ;
#8737 = CIRCLE ( 'NONE', #14580, 20.00000000000000000 ) ;
#8738 = CARTESIAN_POINT ( 'NONE',  ( 11.47554877443044674, 106.3830115231064042, 18.04988257186027312 ) ) ;
#8739 = CARTESIAN_POINT ( 'NONE',  ( -89.61631465359441506, 37.12029293941468211, 10.49999999999999822 ) ) ;
#8740 = EDGE_CURVE ( 'NONE', #10570, #14085, #4413, .T. ) ;
#8741 = LINE ( 'NONE', #12325, #6343 ) ;
#8742 = EDGE_CURVE ( 'NONE', #1839, #14718, #8028, .T. ) ;
#8743 = DIRECTION ( 'NONE',  ( 0.000000000000000000, 0.000000000000000000, 1.000000000000000000 ) ) ;
#8744 = CARTESIAN_POINT ( 'NONE',  ( 0.000000000000000000, 0.000000000000000000, -4.974599999999998801 ) ) ;
#8745 = CIRCLE ( 'NONE', #5598, 7.500000000000001776 ) ;
#8746 = ORIENTED_EDGE ( 'NONE', *, *, #9855, .T. ) ;
#8747 = DIRECTION ( 'NONE',  ( 1.000000000000000000, 0.000000000000000000, 0.000000000000000000 ) ) ;
#8748 = AXIS2_PLACEMENT_3D ( 'NONE', #4324, #10083, #3178 ) ;
#8749 = ORIENTED_EDGE ( 'NONE', *, *, #1813, .T. ) ;
#8750 = CARTESIAN_POINT ( 'NONE',  ( 12.39897948556635754, 73.96800191783272282, -16.00000000000000000 ) ) ;
#8751 = CIRCLE ( 'NONE', #5371, 60.50000000000000000 ) ;
#8752 = CARTESIAN_POINT ( 'NONE',  ( -37.12029293941250074, 89.61631465359532456, -8.000000000000000000 ) ) ;
#8753 = AXIS2_PLACEMENT_3D ( 'NONE', #8374, #6990, #14005 ) ;
#8754 = CARTESIAN_POINT ( 'NONE',  ( 3.999999999999998224, 1.680228229147135544, -3.316631783032547354 ) ) ;
#8755 = ORIENTED_EDGE ( 'NONE', *, *, #7534, .T. ) ;
#8756 = PRODUCT_DEFINITION_SHAPE ( 'NONE', 'NONE',  #898 ) ;
#8757 = ORIENTED_EDGE ( 'NONE', *, *, #8429, .F. ) ;
#8758 = CARTESIAN_POINT ( 'NONE',  ( 0.2500000000000002220, 4.898587196589412829E-16, -4.000000000000000000 ) ) ;
#8759 = ORIENTED_EDGE ( 'NONE', *, *, #2629, .F. ) ;
#8760 = AXIS2_PLACEMENT_3D ( 'NONE', #13804, #1272, #1194 ) ;
#8761 = DIRECTION ( 'NONE',  ( 1.000000000000000000, 0.000000000000000000, 0.000000000000000000 ) ) ;
#8762 = EDGE_CURVE ( 'NONE', #8810, #2149, #1486, .T. ) ;
#8763 = LINE ( 'NONE', #11204, #10233 ) ;
#8764 = EDGE_CURVE ( 'NONE', #406, #3450, #12890, .T. ) ;
#8765 = ORIENTED_EDGE ( 'NONE', *, *, #2686, .T. ) ;
#8766 = CARTESIAN_POINT ( 'NONE',  ( -25.00000000000000000, 81.24038404635962252, -26.00000000000000000 ) ) ;
#8767 = AXIS2_PLACEMENT_3D ( 'NONE', #5506, #955, #2999 ) ;
#8768 = DIRECTION ( 'NONE',  ( 0.000000000000000000, 0.000000000000000000, -1.000000000000000000 ) ) ;
#8769 = DIRECTION ( 'NONE',  ( 6.123233995736766036E-17, 0.000000000000000000, 1.000000000000000000 ) ) ;
#8770 = ORIENTED_EDGE ( 'NONE', *, *, #7118, .T. ) ;
#8771 = ORIENTED_EDGE ( 'NONE', *, *, #3386, .F. ) ;
#8772 = CARTESIAN_POINT ( 'NONE',  ( 25.00000000000000000, 81.24038404635960831, -23.50000000000000000 ) ) ;
#8773 = DIRECTION ( 'NONE',  ( 0.000000000000000000, 0.000000000000000000, 1.000000000000000000 ) ) ;
#8774 = CIRCLE ( 'NONE', #1262, 63.00000000000000000 ) ;
#8775 = DIRECTION ( 'NONE',  ( -0.000000000000000000, -0.000000000000000000, 1.000000000000000000 ) ) ;
#8776 = ORIENTED_EDGE ( 'NONE', *, *, #4264, .T. ) ;
#8777 = CIRCLE ( 'NONE', #12430, 60.50000000000000000 ) ;
#8778 = EDGE_LOOP ( 'NONE', ( #205, #1276, #2728, #8938 ) ) ;
#8779 = EDGE_LOOP ( 'NONE', ( #11501, #893, #13071, #13632 ) ) ;
#8780 = LINE ( 'NONE', #12290, #1807 ) ;
#8781 = VECTOR ( 'NONE', #7002, 1000.000000000000114 ) ;
#8782 = DIRECTION ( 'NONE',  ( 1.000000000000000000, 0.000000000000000000, 0.000000000000000000 ) ) ;
#8783 = DIRECTION ( 'NONE',  ( 0.000000000000000000, 0.000000000000000000, -1.000000000000000000 ) ) ;
#8785 = ORIENTED_EDGE ( 'NONE', *, *, #4824, .F. ) ;
#8784 = ADVANCED_FACE ( 'NONE', ( #413 ), #1695, .F. ) ;
#8786 = FACE_OUTER_BOUND ( 'NONE', #5521, .T. ) ;
#8787 = DIRECTION ( 'NONE',  ( 1.000000000000000000, 0.000000000000000000, 0.000000000000000000 ) ) ;
#8788 = EDGE_CURVE ( 'NONE', #1485, #8869, #5609, .T. ) ;
#8789 = EDGE_LOOP ( 'NONE', ( #13450, #11251, #9742, #4774 ) ) ;
#8790 = DIRECTION ( 'NONE',  ( -0.000000000000000000, -0.000000000000000000, 1.000000000000000000 ) ) ;
#8791 = ORIENTED_EDGE ( 'NONE', *, *, #3620, .F. ) ;
#8792 = CIRCLE ( 'NONE', #72, 60.50000000000000000 ) ;
#8793 = EDGE_LOOP ( 'NONE', ( #11747, #13327, #3277, #1996 ) ) ;
#8794 = CARTESIAN_POINT ( 'NONE',  ( -32.35652065542060285, 95.67730775537752663, 15.49454652436122615 ) ) ;
#8795 = EDGE_CURVE ( 'NONE', #13116, #8815, #6168, .T. ) ;
#8796 = CARTESIAN_POINT ( 'NONE',  ( 0.000000000000000000, 0.000000000000000000, -8.000000000000000000 ) ) ;
#8797 = AXIS2_PLACEMENT_3D ( 'NONE', #9916, #12292, #8782 ) ;
#8798 = PRODUCT_DEFINITION_CONTEXT ( 'detailed design', #5439, 'design' ) ;
#8799 = UNCERTAINTY_MEASURE_WITH_UNIT (LENGTH_MEASURE( 1.000000000000000082E-05 ), #10701, 'distance_accuracy_value', 'NONE');
#8800 = DIRECTION ( 'NONE',  ( 1.000000000000000000, 0.000000000000000000, 0.000000000000000000 ) ) ;
#8801 = DIRECTION ( 'NONE',  ( -0.000000000000000000, -0.000000000000000000, 1.000000000000000000 ) ) ;
#8802 = ADVANCED_FACE ( 'NONE', ( #8595 ), #14375, .F. ) ;
#8803 = CARTESIAN_POINT ( 'NONE',  ( -2.449293598294708880E-16, 38.00000000000000000, -28.00000000000000000 ) ) ;
#8804 = EDGE_CURVE ( 'NONE', #4396, #6265, #14346, .T. ) ;
#8805 = ORIENTED_EDGE ( 'NONE', *, *, #13331, .T. ) ;
#8806 = FACE_BOUND ( 'NONE', #3806, .T. ) ;
#8807 = FACE_OUTER_BOUND ( 'NONE', #234, .T. ) ;
#8808 = CARTESIAN_POINT ( 'NONE',  ( 3.511755186886751368, -2.826662030176382068, -3.597382984111583415 ) ) ;
#8809 = AXIS2_PLACEMENT_3D ( 'NONE', #9508, #8525, #412 ) ;
#8810 = VERTEX_POINT ( 'NONE', #12103 ) ;
#8811 = PLANE ( 'NONE',  #12461 ) ;
#8812 = VERTEX_POINT ( 'NONE', #12261 ) ;
#8813 = CARTESIAN_POINT ( 'NONE',  ( -38.26834323650773229, 92.38795325112918988, 8.000000000000000000 ) ) ;
#8814 = ORIENTED_EDGE ( 'NONE', *, *, #9624, .F. ) ;
#8815 = VERTEX_POINT ( 'NONE', #560 ) ;
#8816 = CYLINDRICAL_SURFACE ( 'NONE', #7881, 3.000000000000002665 ) ;
#8817 = CARTESIAN_POINT ( 'NONE',  ( 0.000000000000000000, 0.000000000000000000, -5.000000000000000888 ) ) ;
#8818 = DIRECTION ( 'NONE',  ( -1.000000000000000000, 0.000000000000000000, 0.000000000000000000 ) ) ;
#8819 = AXIS2_PLACEMENT_3D ( 'NONE', #2062, #3060, #14677 ) ;
#8820 = AXIS2_PLACEMENT_3D ( 'NONE', #9430, #7226, #3682 ) ;
#8821 = DIRECTION ( 'NONE',  ( 1.000000000000000000, 0.000000000000000000, 0.000000000000000000 ) ) ;
#8822 = CARTESIAN_POINT ( 'NONE',  ( 47.21331623427115431, 33.48561063518610581, 8.000000000000000000 ) ) ;
#8823 = DIRECTION ( 'NONE',  ( 0.000000000000000000, 0.000000000000000000, -1.000000000000000000 ) ) ;
#8824 = VERTEX_POINT ( 'NONE', #6385 ) ;
#8825 = CARTESIAN_POINT ( 'NONE',  ( 22.05882352941176094, 71.68269180561141241, -13.50000000000000178 ) ) ;
#8826 = DIRECTION ( 'NONE',  ( 1.000000000000000000, 0.000000000000000000, 0.000000000000000000 ) ) ;
#8827 = DIRECTION ( 'NONE',  ( -1.000000000000000000, 0.000000000000000000, 0.000000000000000000 ) ) ;
#8828 = AXIS2_PLACEMENT_3D ( 'NONE', #7096, #12745, #2265 ) ;
#8829 = CIRCLE ( 'NONE', #10047, 4.250000000000000000 ) ;
#8830 = ORIENTED_EDGE ( 'NONE', *, *, #12301, .T. ) ;
#8831 = ORIENTED_EDGE ( 'NONE', *, *, #2407, .T. ) ;
#8832 = CARTESIAN_POINT ( 'NONE',  ( 0.000000000000000000, 0.000000000000000000, 14.49999999999999822 ) ) ;
#8833 = ORIENTED_EDGE ( 'NONE', *, *, #5240, .F. ) ;
#8834 = FACE_OUTER_BOUND ( 'NONE', #2581, .T. ) ;
#8835 = CARTESIAN_POINT ( 'NONE',  ( 0.000000000000000000, 0.000000000000000000, 0.000000000000000000 ) ) ;
#8836 = ORIENTED_EDGE ( 'NONE', *, *, #12347, .F. ) ;
#8837 = CIRCLE ( 'NONE', #3762, 60.50000000000000000 ) ;
#8838 = CARTESIAN_POINT ( 'NONE',  ( -52.50000000000000711, 0.000000000000000000, -13.00000000000000178 ) ) ;
#8839 = DIRECTION ( 'NONE',  ( 0.000000000000000000, 0.000000000000000000, 1.000000000000000000 ) ) ;
#8840 = CARTESIAN_POINT ( 'NONE',  ( -22.33583958711380646, -30.74264578624812927, 19.49999999999999645 ) ) ;
#8841 = ORIENTED_EDGE ( 'NONE', *, *, #1657, .T. ) ;
#8842 = AXIS2_PLACEMENT_3D ( 'NONE', #11975, #8394, #8681 ) ;
#8843 = VECTOR ( 'NONE', #12182, 1000.000000000000000 ) ;
#8844 = AXIS2_PLACEMENT_3D ( 'NONE', #6750, #11409, #9119 ) ;
#8845 = ORIENTED_EDGE ( 'NONE', *, *, #1979, .T. ) ;
#8846 = CARTESIAN_POINT ( 'NONE',  ( 27.94117647058824616, 90.79807628710781842, 13.50000000000000533 ) ) ;
#8847 = DIRECTION ( 'NONE',  ( -0.000000000000000000, -0.000000000000000000, 1.000000000000000000 ) ) ;
#8848 = ADVANCED_FACE ( 'NONE', ( #6235 ), #12178, .F. ) ;
#8849 = FACE_OUTER_BOUND ( 'NONE', #5291, .T. ) ;
#8850 = EDGE_CURVE ( 'NONE', #13430, #12536, #6048, .T. ) ;
#8852 = VERTEX_POINT ( 'NONE', #6613 ) ;
#8851 = EDGE_CURVE ( 'NONE', #5997, #5159, #4903, .T. ) ;
#8853 = AXIS2_PLACEMENT_3D ( 'NONE', #10172, #5841, #8954 ) ;
#8854 = ORIENTED_EDGE ( 'NONE', *, *, #5225, .T. ) ;
#8855 = AXIS2_PLACEMENT_3D ( 'NONE', #7032, #9175, #13902 ) ;
#8856 = VERTEX_POINT ( 'NONE', #711 ) ;
#8857 = EDGE_CURVE ( 'NONE', #12316, #6659, #10467, .T. ) ;
#8858 = CARTESIAN_POINT ( 'NONE',  ( 0.2500000000000002220, 0.000000000000000000, 0.000000000000000000 ) ) ;
#8859 = ADVANCED_FACE ( 'NONE', ( #1915 ), #5338, .T. ) ;
#8860 = LINE ( 'NONE', #825, #1291 ) ;
#8861 = DIRECTION ( 'NONE',  ( -1.000000000000000000, 0.000000000000000000, 0.000000000000000000 ) ) ;
#8862 = AXIS2_PLACEMENT_3D ( 'NONE', #1720, #6325, #10982 ) ;
#8863 = ORIENTED_EDGE ( 'NONE', *, *, #1243, .F. ) ;
#8864 = CIRCLE ( 'NONE', #4018, 60.50000000000000000 ) ;
#8865 = DIRECTION ( 'NONE',  ( 1.000000000000000000, 0.000000000000000000, 0.000000000000000000 ) ) ;
#8866 = CARTESIAN_POINT ( 'NONE',  ( -34.09759333678486115, 101.2734996710205451, 15.50321023462188030 ) ) ;
#8867 = ORIENTED_EDGE ( 'NONE', *, *, #602, .T. ) ;
#8868 = DIRECTION ( 'NONE',  ( 0.000000000000000000, 0.000000000000000000, 1.000000000000000000 ) ) ;
#8869 = VERTEX_POINT ( 'NONE', #3293 ) ;
#8870 = ORIENTED_EDGE ( 'NONE', *, *, #9127, .T. ) ;
#8871 = CARTESIAN_POINT ( 'NONE',  ( 56.43380494353997534, 12.86891638962136319, -10.50000000000000000 ) ) ;
#8872 = CIRCLE ( 'NONE', #11803, 3.000000000000002665 ) ;
#8873 = EDGE_CURVE ( 'NONE', #9553, #8704, #3198, .T. ) ;
#8874 = CARTESIAN_POINT ( 'NONE',  ( 0.000000000000000000, 0.000000000000000000, -10.50000000000000000 ) ) ;
#8875 = DIRECTION ( 'NONE',  ( 0.000000000000000000, 0.000000000000000000, 1.000000000000000000 ) ) ;
#8876 = CARTESIAN_POINT ( 'NONE',  ( 0.000000000000000000, 0.000000000000000000, -8.000000000000000000 ) ) ;
#8877 = DIRECTION ( 'NONE',  ( -0.000000000000000000, -0.000000000000000000, 1.000000000000000000 ) ) ;
#8878 = ORIENTED_EDGE ( 'NONE', *, *, #6824, .T. ) ;
#8879 = CIRCLE ( 'NONE', #9601, 52.50000000000000711 ) ;
#8880 = CARTESIAN_POINT ( 'NONE',  ( 31.95997502295791648, -41.65105036528979099, -10.50000000000000000 ) ) ;
#8881 = CYLINDRICAL_SURFACE ( 'NONE', #5974, 3.000000000000002665 ) ;
#8882 = DIRECTION ( 'NONE',  ( 1.000000000000000000, 0.000000000000000000, 0.000000000000000000 ) ) ;
#8883 = ORIENTED_EDGE ( 'NONE', *, *, #3646, .F. ) ;
#8884 = CARTESIAN_POINT ( 'NONE',  ( 100.0000000000000000, -1.224646799147353217E-14, -13.00000000000000178 ) ) ;
#8885 = VERTEX_POINT ( 'NONE', #7979 ) ;
#8886 = EDGE_CURVE ( 'NONE', #13653, #967, #11697, .T. ) ;
#8887 = DIRECTION ( 'NONE',  ( 0.000000000000000000, 0.000000000000000000, 1.000000000000000000 ) ) ;
#8888 = EDGE_CURVE ( 'NONE', #508, #5898, #10705, .T. ) ;
#8889 = ORIENTED_EDGE ( 'NONE', *, *, #2435, .F. ) ;
#8890 = CARTESIAN_POINT ( 'NONE',  ( 0.000000000000000000, 0.000000000000000000, 8.000000000000000000 ) ) ;
#8891 = ORIENTED_EDGE ( 'NONE', *, *, #6230, .F. ) ;
#8892 = ORIENTED_EDGE ( 'NONE', *, *, #13575, .F. ) ;
#8893 = CYLINDRICAL_SURFACE ( 'NONE', #121, 2.500000000000000444 ) ;
#8894 = CARTESIAN_POINT ( 'NONE',  ( 5.204748896376250896E-15, 85.00000000000000000, 46.00000000000000000 ) ) ;
#8895 = FACE_OUTER_BOUND ( 'NONE', #13038, .T. ) ;
#8896 = DIRECTION ( 'NONE',  ( 1.000000000000000000, 0.000000000000000000, 0.000000000000000000 ) ) ;
#8897 = DIRECTION ( 'NONE',  ( -1.000000000000000000, 0.000000000000000000, 0.000000000000000000 ) ) ;
#8898 = EDGE_CURVE ( 'NONE', #10917, #2326, #7911, .T. ) ;
#8899 = DIRECTION ( 'NONE',  ( 0.000000000000000000, 0.000000000000000000, 1.000000000000000000 ) ) ;
#8900 = ORIENTED_EDGE ( 'NONE', *, *, #1067, .T. ) ;
#8901 = CARTESIAN_POINT ( 'NONE',  ( 12.28339058173379783, 73.98737765342407613, -16.56626766863480782 ) ) ;
#8902 = CARTESIAN_POINT ( 'NONE',  ( 12.39897948556635754, 94.18739463280904545, -16.00000000000000000 ) ) ;
#8903 = DIRECTION ( 'NONE',  ( -1.000000000000000000, 0.000000000000000000, 0.000000000000000000 ) ) ;
#8904 = DIRECTION ( 'NONE',  ( -0.000000000000000000, -0.000000000000000000, 1.000000000000000000 ) ) ;
#8905 = EDGE_CURVE ( 'NONE', #7460, #7720, #4175, .T. ) ;
#8906 = VERTEX_POINT ( 'NONE', #13607 ) ;
#8907 = CARTESIAN_POINT ( 'NONE',  ( -1.274258131565023877, -3.883108878240887130, -3.220599429844052342 ) ) ;
#8908 = EDGE_LOOP ( 'NONE', ( #9874, #14044 ) ) ;
#8909 = CARTESIAN_POINT ( 'NONE',  ( -51.53979475227126983, -13.35619814848815601, -13.00000000000000178 ) ) ;
#8910 = DIRECTION ( 'NONE',  ( -0.000000000000000000, -0.000000000000000000, -1.000000000000000000 ) ) ;
#8911 = CLOSED_SHELL ( 'NONE', ( #8784, #6331, #11842, #1417, #7685, #644, #3141, #14766, #9532, #976, #14562, #6153, #7304, #5467, #13502, #6731, #8391, #7673, #5431, #13335, #14924, #3940, #3775, #10387, #7788, #9309, #11110, #6429, #6439, #5774, #14928, #13483, #1339, #14750, #4637, #7691, #14020, #6351, #14473, #6238, #9445, #5755, #13079, #598, #7482, #5241, #9891, #13605, #10880, #7655, #9169, #6909, #4782, #3337, #14426, #4310, #5456, #4721, #9831, #3435, #4974, #10288, #12791, #14067, #11824, #10241, #410, #10303, #5655, #12204, #14176, #2213, #14941, #11788, #8029, #14981, #3855, #6002, #4683, #789, #4633, #13979, #9903, #4536, #14372, #4071, #11497, #3642, #4371, #1050, #3898, #2317, #6468, #10911, #11936, #11000, #8654, #4954, #11405, #3059, #9580, #11590, #2069, #10853, #4907, #9168, #4905, #7725, #12939, #1889, #1998, #13002, #3148, #7676, #13218, #10295, #4283, #3860, #3664, #1359, #6733, #12688, #7906, #13072, #9308, #2638, #11137, #4313, #791, #5606, #365, #1769, #6557, #5921, #3116, #11086, #8612, #9225, #12329, #7288, #1708, #6829, #6194, #10882, #724, #2735, #7094, #10170, #129, #2355, #3809, #2525, #13522, #9576, #4273, #8009, #11610, #718, #14897, #5294, #12425, #9250, #209, #8653, #6518, #8193, #13783, #1457, #3144, #14327, #11797, #2280, #8347, #2719, #8693, #2388, #6246, #1561, #4930, #4861, #11642, #1337, #10175, #14110, #7944, #9492, #11403, #11114, #7219, #14463, #741, #10888, #4859, #9267, #5048, #4591, #9940, #11570, #3876, #10939, #3802, #4238, #2299, #14658, #10744, #13844, #9671, #7831, #2218, #9494, #7496, #6000, #4220, #13503, #14047, #11499, #4816, #10984, #13810, #6435, #6061, #9913, #4195, #447, #2310, #6969, #1484, #1193, #2944, #2087, #8848, #1853, #10557, #5551, #834, #9369, #14179, #10634, #322, #3607, #4409, #11833, #7776, #12751, #3566, #13436, #6152, #13888, #1540, #1648, #12387, #10513, #12578, #2477, #10532, #920, #3424, #6749, #10650, #5919, #14996, #1254, #186, #12598, #10097, #14100, #10470, #8256, #14381, #5515, #13529, #2164, #7314, #548, #13881, #13171, #14983, #11084, #1152, #9319, #9075, #8802, #6330 ) ) ;
#8912 = CARTESIAN_POINT ( 'NONE',  ( 10.00086283267470932, 106.5319533799504654, -19.34189422912923462 ) ) ;
#8913 = LINE ( 'NONE', #12195, #66 ) ;
#8914 = ORIENTED_EDGE ( 'NONE', *, *, #1431, .F. ) ;
#8915 = ORIENTED_EDGE ( 'NONE', *, *, #3245, .T. ) ;
#8916 = ORIENTED_EDGE ( 'NONE', *, *, #13694, .F. ) ;
#8917 = CARTESIAN_POINT ( 'NONE',  ( -36.70371619500578220, -89.33979373934407420, -10.50000000000000000 ) ) ;
#8918 = CARTESIAN_POINT ( 'NONE',  ( 72.70695371924547601, 57.06275842387054098, 8.000000000000000000 ) ) ;
#8919 = DIRECTION ( 'NONE',  ( 1.000000000000000000, 0.000000000000000000, 0.000000000000000000 ) ) ;
#8920 = EDGE_LOOP ( 'NONE', ( #8034, #7594, #6727, #9967, #3418, #10592 ) ) ;
#8921 = VERTEX_POINT ( 'NONE', #9044 ) ;
#8922 = VERTEX_POINT ( 'NONE', #13465 ) ;
#8923 = DIRECTION ( 'NONE',  ( -0.000000000000000000, -0.000000000000000000, 1.000000000000000000 ) ) ;
#8924 = FACE_OUTER_BOUND ( 'NONE', #4788, .T. ) ;
#8925 = EDGE_CURVE ( 'NONE', #2119, #6659, #8970, .T. ) ;
#8926 = DIRECTION ( 'NONE',  ( 0.000000000000000000, 0.000000000000000000, 1.000000000000000000 ) ) ;
#8927 = EDGE_CURVE ( 'NONE', #6973, #2752, #3442, .T. ) ;
#8928 = ORIENTED_EDGE ( 'NONE', *, *, #10192, .T. ) ;
#8929 = DIRECTION ( 'NONE',  ( -0.000000000000000000, -0.000000000000000000, 1.000000000000000000 ) ) ;
#8930 = DIRECTION ( 'NONE',  ( 0.000000000000000000, 0.000000000000000000, -1.000000000000000000 ) ) ;
#8931 = ORIENTED_EDGE ( 'NONE', *, *, #8485, .T. ) ;
#8932 = CARTESIAN_POINT ( 'NONE',  ( 3.680118525130242180, -2.494084732383343272, -0.3507732604232501328 ) ) ;
#8933 = ORIENTED_EDGE ( 'NONE', *, *, #4269, .T. ) ;
#8934 = EDGE_CURVE ( 'NONE', #6576, #479, #5140, .T. ) ;
#8935 = ORIENTED_EDGE ( 'NONE', *, *, #12727, .T. ) ;
#8936 = CARTESIAN_POINT ( 'NONE',  ( 0.000000000000000000, 0.000000000000000000, 14.49999999999999822 ) ) ;
#8937 = PRODUCT_DEFINITION ( 'UNKNOWN', '', #2184, #14586 ) ;
#8938 = ORIENTED_EDGE ( 'NONE', *, *, #5337, .F. ) ;
#8939 = CARTESIAN_POINT ( 'NONE',  ( 53.63365512954693770, -9.714003807513686084, -13.00000000000000178 ) ) ;
#8940 = CIRCLE ( 'NONE', #2167, 3.000000000000002665 ) ;
#8941 = CARTESIAN_POINT ( 'NONE',  ( 2.500000000000002220, 6.938893903907228378E-15, 2.042000000000002036 ) ) ;
#8942 = DIRECTION ( 'NONE',  ( 1.000000000000000000, 0.000000000000000000, 0.000000000000000000 ) ) ;
#8943 = DIRECTION ( 'NONE',  ( -1.000000000000000000, 0.000000000000000000, 0.000000000000000000 ) ) ;
#8944 = EDGE_CURVE ( 'NONE', #11984, #12052, #5619, .T. ) ;
#8945 = B_SPLINE_CURVE_WITH_KNOTS ( 'NONE', 3,
 ( #3628, #854, #10603, #2056, #137, #201, #9027, #9112, #3196, #3275 ),
 .UNSPECIFIED., .F., .F.,
 ( 4, 2, 2, 2, 4 ),
 ( 0.000000000000000000, 0.001715760189696190381, 0.003431520379392380762, 0.005147280569088571144, 0.006863040758784761525 ),
 .UNSPECIFIED. ) ;
#8946 = CARTESIAN_POINT ( 'NONE',  ( 5.000000000000007994, 0.000000000000000000, 4.250000000000028422 ) ) ;
#8947 = VERTEX_POINT ( 'NONE', #10116 ) ;
#8948 = COLOUR_RGB ( '', 0.66274510, 0.83137255, 0.94901961) ;
#8949 = FACE_OUTER_BOUND ( 'NONE', #1907, .T. ) ;
#8950 = DIRECTION ( 'NONE',  ( -1.000000000000000000, 0.000000000000000000, 0.000000000000000000 ) ) ;
#8951 = AXIS2_PLACEMENT_3D ( 'NONE', #7810, #5247, #14664 ) ;
#8952 = CARTESIAN_POINT ( 'NONE',  ( -2.804994570502170603, -3.229033611042463114, -3.526374918436837813 ) ) ;
#8953 = ORIENTED_EDGE ( 'NONE', *, *, #11695, .F. ) ;
#8954 = DIRECTION ( 'NONE',  ( 1.000000000000000000, 0.000000000000000000, 0.000000000000000000 ) ) ;
#8955 = ORIENTED_EDGE ( 'NONE', *, *, #699, .F. ) ;
#8956 = CARTESIAN_POINT ( 'NONE',  ( 0.000000000000000000, 0.000000000000000000, -13.00000000000000178 ) ) ;
#8957 = ORIENTED_EDGE ( 'NONE', *, *, #7554, .T. ) ;
#8958 = CARTESIAN_POINT ( 'NONE',  ( 0.000000000000000000, 0.000000000000000000, 16.00000000000000000 ) ) ;
#8959 = AXIS2_PLACEMENT_3D ( 'NONE', #9577, #10726, #2753 ) ;
#8960 = DIRECTION ( 'NONE',  ( -1.000000000000000000, 0.000000000000000000, 0.000000000000000000 ) ) ;
#8962 = CARTESIAN_POINT ( 'NONE',  ( -1.747541505913279947, 3.837784562140252653, -3.503702292528905637 ) ) ;
#8961 = AXIS2_PLACEMENT_3D ( 'NONE', #3979, #7225, #9725 ) ;
#8963 = DIRECTION ( 'NONE',  ( 0.000000000000000000, 0.000000000000000000, 1.000000000000000000 ) ) ;
#8964 = MANIFOLD_SOLID_BREP ( 'Cavity1', #4074 ) ;
#8965 = AXIS2_PLACEMENT_3D ( 'NONE', #5109, #9722, #13162 ) ;
#8966 = CARTESIAN_POINT ( 'NONE',  ( 13.71740939043365337, -51.19406879332061067, 10.49999999999999822 ) ) ;
#8968 = CARTESIAN_POINT ( 'NONE',  ( 7.500000000000000888, 59.24038404635959409, -15.00000000000000355 ) ) ;
#8967 = VECTOR ( 'NONE', #5395, 1000.000000000000000 ) ;
#8969 = EDGE_CURVE ( 'NONE', #8073, #5446, #9724, .T. ) ;
#8970 = LINE ( 'NONE', #4291, #13140 ) ;
#8971 = EDGE_CURVE ( 'NONE', #13514, #2375, #12843, .T. ) ;
#8972 = ORIENTED_EDGE ( 'NONE', *, *, #10202, .T. ) ;
#8973 = EDGE_CURVE ( 'NONE', #14518, #7413, #8774, .T. ) ;
#8974 = DIRECTION ( 'NONE',  ( 0.000000000000000000, 0.000000000000000000, 1.000000000000000000 ) ) ;
#8975 = CARTESIAN_POINT ( 'NONE',  ( 52.54657765281197612, -6.917888187662545540, 8.000000000000000000 ) ) ;
#8976 = EDGE_CURVE ( 'NONE', #7044, #12589, #9008, .T. ) ;
#8977 = DIRECTION ( 'NONE',  ( 1.000000000000000000, 0.000000000000000000, 0.000000000000000000 ) ) ;
#8978 = CIRCLE ( 'NONE', #2431, 53.55662432702593634 ) ;
#8979 = DIRECTION ( 'NONE',  ( 0.000000000000000000, 0.000000000000000000, -1.000000000000000000 ) ) ;
#8980 = EDGE_LOOP ( 'NONE', ( #9751, #6624, #2423, #11664 ) ) ;
#8981 = EDGE_CURVE ( 'NONE', #6713, #1920, #2464, .T. ) ;
#8982 = DIRECTION ( 'NONE',  ( 0.000000000000000000, 0.000000000000000000, -1.000000000000000000 ) ) ;
#8983 = VERTEX_POINT ( 'NONE', #2436 ) ;
#8984 = DIRECTION ( 'NONE',  ( 1.000000000000000000, 0.000000000000000000, 0.000000000000000000 ) ) ;
#8985 = FACE_OUTER_BOUND ( 'NONE', #41, .T. ) ;
#8986 = AXIS2_PLACEMENT_3D ( 'NONE', #3716, #10608, #4015 ) ;
#8987 = CARTESIAN_POINT ( 'NONE',  ( 11.99124924651180102, 106.3260354126052363, -17.22144562113022204 ) ) ;
#8988 = DIRECTION ( 'NONE',  ( 0.000000000000000000, 0.000000000000000000, 1.000000000000000000 ) ) ;
#8989 = SHAPE_DEFINITION_REPRESENTATION ( #13369, #10623 ) ;
#8990 = ORIENTED_EDGE ( 'NONE', *, *, #13914, .F. ) ;
#8991 = CIRCLE ( 'NONE', #10933, 3.000000000000002665 ) ;
#8992 = ORIENTED_EDGE ( 'NONE', *, *, #2545, .F. ) ;
#8993 = VERTEX_POINT ( 'NONE', #1097 ) ;
#8994 = ADVANCED_FACE ( 'NONE', ( #88, #10632 ), #3519, .T. ) ;
#8995 = AXIS2_PLACEMENT_3D ( 'NONE', #13207, #9846, #8418 ) ;
#8996 = DIRECTION ( 'NONE',  ( -1.000000000000000000, 0.000000000000000000, 0.000000000000000000 ) ) ;
#8997 = CARTESIAN_POINT ( 'NONE',  ( 33.83495342806090633, 101.3902949203995689, 15.35262818605211699 ) ) ;
#8998 = DIRECTION ( 'NONE',  ( -1.000000000000000000, -0.000000000000000000, -0.000000000000000000 ) ) ;
#8999 = ORIENTED_EDGE ( 'NONE', *, *, #6018, .T. ) ;
#9000 = AXIS2_PLACEMENT_3D ( 'NONE', #4547, #9306, #6952 ) ;
#9001 = ORIENTED_EDGE ( 'NONE', *, *, #9855, .F. ) ;
#9002 = ORIENTED_EDGE ( 'NONE', *, *, #10427, .F. ) ;
#9003 = CIRCLE ( 'NONE', #1491, 2.041999999999999815 ) ;
#9004 = DIRECTION ( 'NONE',  ( 0.000000000000000000, 0.000000000000000000, 1.000000000000000000 ) ) ;
#9005 = FACE_OUTER_BOUND ( 'NONE', #12210, .T. ) ;
#9006 = CARTESIAN_POINT ( 'NONE',  ( 0.000000000000000000, 0.000000000000000000, -13.00000000000000178 ) ) ;
#9008 = CIRCLE ( 'NONE', #40, 0.5000000000000038858 ) ;
#9007 = DIRECTION ( 'NONE',  ( 1.000000000000000000, 6.308085367188385311E-16, 0.000000000000000000 ) ) ;
#9009 = DIRECTION ( 'NONE',  ( 0.000000000000000000, 0.000000000000000000, -1.000000000000000000 ) ) ;
#9010 = ORIENTED_EDGE ( 'NONE', *, *, #12875, .F. ) ;
#9011 = CARTESIAN_POINT ( 'NONE',  ( 2.500000000000002220, -1.178949249685222522, -2.042000000000002036 ) ) ;
#9012 = CIRCLE ( 'NONE', #8528, 60.49999999999999289 ) ;
#9013 = ORIENTED_EDGE ( 'NONE', *, *, #5082, .F. ) ;
#9014 = EDGE_LOOP ( 'NONE', ( #9649, #1261, #5311, #9996, #3169 ) ) ;
#9015 = DIRECTION ( 'NONE',  ( 1.000000000000000000, 0.000000000000000000, 0.000000000000000000 ) ) ;
#9016 = EDGE_CURVE ( 'NONE', #2530, #2568, #5711, .T. ) ;
#9017 = VECTOR ( 'NONE', #38, 1000.000000000000000 ) ;
#9018 = CARTESIAN_POINT ( 'NONE',  ( 32.26435573746228158, -42.04772703543541468, -13.00000000000000178 ) ) ;
#9019 = CARTESIAN_POINT ( 'NONE',  ( 26.99988008862626643, 45.88839665196127271, 10.49999999999999822 ) ) ;
#9020 = AXIS2_PLACEMENT_3D ( 'NONE', #9140, #10504, #1033 ) ;
#9021 = LINE ( 'NONE', #11161, #4989 ) ;
#9022 = CARTESIAN_POINT ( 'NONE',  ( 0.1404048886732826851, 4.699864953788067901, -3.686887068327037831 ) ) ;
#9023 = DIRECTION ( 'NONE',  ( -0.000000000000000000, -0.000000000000000000, 1.000000000000000000 ) ) ;
#9024 = VERTEX_POINT ( 'NONE', #7057 ) ;
#9025 = DIRECTION ( 'NONE',  ( 1.000000000000000000, 0.000000000000000000, 0.000000000000000000 ) ) ;
#9026 = VECTOR ( 'NONE', #715, 1000.000000000000114 ) ;
#9027 = CARTESIAN_POINT ( 'NONE',  ( 11.47656068366043414, 61.94660012053729048, 18.08543280684388321 ) ) ;
#9028 = CARTESIAN_POINT ( 'NONE',  ( 1.747541505913281279, -3.837784562140267308, -3.503702292528909190 ) ) ;
#9029 = EDGE_CURVE ( 'NONE', #11449, #10669, #3690, .T. ) ;
#9030 = ORIENTED_EDGE ( 'NONE', *, *, #507, .F. ) ;
#9031 = CARTESIAN_POINT ( 'NONE',  ( -22.05882352941176450, 71.68269180561142662, -13.50000000000000178 ) ) ;
#9032 = EDGE_CURVE ( 'NONE', #13122, #7998, #11717, .T. ) ;
#9033 = EDGE_CURVE ( 'NONE', #5812, #13295, #2957, .T. ) ;
#9034 = AXIS2_PLACEMENT_3D ( 'NONE', #5957, #14312, #7320 ) ;
#9035 = FACE_OUTER_BOUND ( 'NONE', #6763, .T. ) ;
#9036 = EDGE_CURVE ( 'NONE', #9073, #11672, #1031, .T. ) ;
#9037 = DIRECTION ( 'NONE',  ( 0.000000000000000000, 0.000000000000000000, -1.000000000000000000 ) ) ;
#9038 = AXIS2_PLACEMENT_3D ( 'NONE', #3346, #7964, #1358 ) ;
#9039 = CARTESIAN_POINT ( 'NONE',  ( 5.000000000000006217, 3.306546357697854226E-16, 2.700000000000028155 ) ) ;
#9040 = DIRECTION ( 'NONE',  ( -1.000000000000000000, 0.000000000000000000, 0.000000000000000000 ) ) ;
#9041 = PLANE ( 'NONE',  #14616 ) ;
#9042 = DIRECTION ( 'NONE',  ( 0.000000000000000000, 0.000000000000000000, 1.000000000000000000 ) ) ;
#9043 = CARTESIAN_POINT ( 'NONE',  ( 2.500000000000000444, 0.000000000000000000, -5.000000000000000888 ) ) ;
#9044 = CARTESIAN_POINT ( 'NONE',  ( -33.49014761921589667, 11.74264578624790190, -28.00000000000000000 ) ) ;
#9045 = AXIS2_PLACEMENT_3D ( 'NONE', #9213, #6856, #13711 ) ;
#9046 = ORIENTED_EDGE ( 'NONE', *, *, #4079, .T. ) ;
#9047 = CARTESIAN_POINT ( 'NONE',  ( 5.384454397937118664, 0.000000000000000000, -4.484454397937119197 ) ) ;
#9048 = CARTESIAN_POINT ( 'NONE',  ( 11.46115996437298712, 94.30629603967057051, -18.06445797889986338 ) ) ;
#9049 = VECTOR ( 'NONE', #668, 1000.000000000000000 ) ;
#9050 = DIRECTION ( 'NONE',  ( 1.000000000000000000, 0.000000000000000000, 0.000000000000000000 ) ) ;
#9051 = DIRECTION ( 'NONE',  ( 0.000000000000000000, 0.000000000000000000, 1.000000000000000000 ) ) ;
#9052 = VERTEX_POINT ( 'NONE', #2516 ) ;
#9053 = CIRCLE ( 'NONE', #11511, 3.000000000000002665 ) ;
#9054 = FACE_OUTER_BOUND ( 'NONE', #9077, .T. ) ;
#9055 = AXIS2_PLACEMENT_3D ( 'NONE', #5980, #12904, #11774 ) ;
#9056 = ORIENTED_EDGE ( 'NONE', *, *, #5096, .F. ) ;
#9057 = EDGE_CURVE ( 'NONE', #1886, #7929, #11933, .T. ) ;
#9058 = DIRECTION ( 'NONE',  ( 1.000000000000000000, 0.000000000000000000, 0.000000000000000000 ) ) ;
#9059 = CARTESIAN_POINT ( 'NONE',  ( -13.71740939043329277, 51.19406879332069593, 10.49999999999999822 ) ) ;
#9060 = EDGE_CURVE ( 'NONE', #6775, #12166, #8038, .T. ) ;
#9061 = DIRECTION ( 'NONE',  ( 1.000000000000000000, 0.000000000000000000, 0.000000000000000000 ) ) ;
#9062 = CARTESIAN_POINT ( 'NONE',  ( 47.00000000000001421, 81.24038404635960831, 31.00000000000000000 ) ) ;
#9063 = VERTEX_POINT ( 'NONE', #9274 ) ;
#9064 = VERTEX_POINT ( 'NONE', #10568 ) ;
#9065 = AXIS2_PLACEMENT_3D ( 'NONE', #875, #1020, #1918 ) ;
#9066 = ORIENTED_EDGE ( 'NONE', *, *, #11523, .F. ) ;
#9067 = VECTOR ( 'NONE', #10625, 1000.000000000000000 ) ;
#9068 = DIRECTION ( 'NONE',  ( 1.000000000000000000, 0.000000000000000000, 0.000000000000000000 ) ) ;
#9069 = CARTESIAN_POINT ( 'NONE',  ( 12.39897948556635576, 94.18739463280904545, 16.00000000000000000 ) ) ;
#9070 = AXIS2_PLACEMENT_3D ( 'NONE', #10300, #3323, #2104 ) ;
#9071 =( BOUNDED_SURFACE ( )  B_SPLINE_SURFACE ( 3, 2, ( 
 ( #6469, #4137, #566 ),
 ( #11272, #876, #13471 ),
 ( #2992, #13392, #13314 ),
 ( #11119, #6539, #4362 ),
 ( #8754, #7615, #11197 ),
 ( #13613, #6390, #1701 ) ),
 .UNSPECIFIED., .F., .F., .T. ) 
 B_SPLINE_SURFACE_WITH_KNOTS ( ( 4, 2, 4 ),
 ( 3, 3 ),
 ( 0.02027065861071770947, 0.02273072267836921331, 0.02519078674602071716 ),
 ( 0.000000000000000000, 1.000000000000000000 ),
 .UNSPECIFIED. ) 
 GEOMETRIC_REPRESENTATION_ITEM ( )  RATIONAL_B_SPLINE_SURFACE ( (
 ( 1.000000000000000000, 0.8047781708337298223, 1.000000000000000000),
 ( 1.000000000000000000, 0.8123765190704248518, 1.000000000000000000),
 ( 1.000000000000000000, 0.8190656277165397903, 1.000000000000000000),
 ( 1.000000000000000000, 0.8192366903510730491, 1.000000000000000000),
 ( 1.000000000000000000, 0.8126138454303968306, 1.000000000000000000),
 ( 1.000000000000000000, 0.8047712246031420991, 1.000000000000000000) ) ) 
 REPRESENTATION_ITEM ( '' )  SURFACE ( )  );
#9072 = CARTESIAN_POINT ( 'NONE',  ( -3.999999999999996447, -2.309401076758518911, -0.5000000000000004441 ) ) ;
#9073 = VERTEX_POINT ( 'NONE', #7138 ) ;
#9074 = EDGE_LOOP ( 'NONE', ( #5597, #13866 ) ) ;
#9075 = ADVANCED_FACE ( 'NONE', ( #14985 ), #4735, .F. ) ;
#9076 = CIRCLE ( 'NONE', #13953, 17.00000000000001066 ) ;
#9077 = EDGE_LOOP ( 'NONE', ( #10802, #1718, #5042, #3705 ) ) ;
#9078 = EDGE_CURVE ( 'NONE', #5604, #1589, #5383, .T. ) ;
#9079 = AXIS2_PLACEMENT_3D ( 'NONE', #12191, #1711, #4072 ) ;
#9080 = DIRECTION ( 'NONE',  ( 0.000000000000000000, 0.000000000000000000, -1.000000000000000000 ) ) ;
#9081 = AXIS2_PLACEMENT_3D ( 'NONE', #13526, #5487, #3130 ) ;
#9082 = PLANE ( 'NONE',  #6306 ) ;
#9083 = DIRECTION ( 'NONE',  ( -0.000000000000000000, -0.000000000000000000, -1.000000000000000000 ) ) ;
#9084 = SHAPE_REPRESENTATION_RELATIONSHIP ( 'NONE' , 'NONE' ,  #10623, #2938 ) ;
#9085 = DIRECTION ( 'NONE',  ( 0.000000000000000000, -0.5000000000000008882, -0.8660254037844380415 ) ) ;
#9086 = ORIENTED_EDGE ( 'NONE', *, *, #2629, .T. ) ;
#9087 = CARTESIAN_POINT ( 'NONE',  ( 68.49330278050122445, -68.09867107463004743, 10.49999999999999822 ) ) ;
#9088 = EDGE_LOOP ( 'NONE', ( #10837, #10149, #3530, #9707, #7797, #13110, #13641 ) ) ;
#9089 = ORIENTED_EDGE ( 'NONE', *, *, #8150, .T. ) ;
#9090 = EDGE_CURVE ( 'NONE', #1620, #5654, #4665, .T. ) ;
#9091 = DIRECTION ( 'NONE',  ( 0.000000000000000000, 0.000000000000000000, 1.000000000000000000 ) ) ;
#9092 = DIRECTION ( 'NONE',  ( 1.000000000000000000, 0.000000000000000000, 0.000000000000000000 ) ) ;
#9093 = AXIS2_PLACEMENT_3D ( 'NONE', #9261, #6679, #5766 ) ;
#9094 = CIRCLE ( 'NONE', #12986, 3.000000000000002665 ) ;
#9095 = EDGE_LOOP ( 'NONE', ( #11862, #12019, #12337, #4642 ) ) ;
#9096 = AXIS2_PLACEMENT_3D ( 'NONE', #11622, #1211, #12759 ) ;
#9097 = ORIENTED_EDGE ( 'NONE', *, *, #13546, .F. ) ;
#9098 = DIRECTION ( 'NONE',  ( 0.000000000000000000, 0.000000000000000000, 1.000000000000000000 ) ) ;
#9099 = ORIENTED_EDGE ( 'NONE', *, *, #2217, .F. ) ;
#9100 = ORIENTED_EDGE ( 'NONE', *, *, #6929, .F. ) ;
#9101 = CIRCLE ( 'NONE', #7650, 52.50000000000000711 ) ;
#9102 = DIRECTION ( 'NONE',  ( 1.000000000000000000, 0.000000000000000000, 0.000000000000000000 ) ) ;
#9103 = DIRECTION ( 'NONE',  ( 1.000000000000000000, 0.000000000000000000, 0.000000000000000000 ) ) ;
#9104 = AXIS2_PLACEMENT_3D ( 'NONE', #3335, #2117, #12528 ) ;
#9105 = DIRECTION ( 'NONE',  ( 0.000000000000000000, 0.000000000000000000, -1.000000000000000000 ) ) ;
#9106 = FACE_OUTER_BOUND ( 'NONE', #6228, .T. ) ;
#9107 = CARTESIAN_POINT ( 'NONE',  ( -25.00000000000000000, 81.24038404635962252, 16.00000000000000000 ) ) ;
#9108 = ORIENTED_EDGE ( 'NONE', *, *, #7325, .T. ) ;
#9109 = CARTESIAN_POINT ( 'NONE',  ( 46.63108361037843252, 56.43380494353993271, -13.00000000000000178 ) ) ;
#9110 = VERTEX_POINT ( 'NONE', #3742 ) ;
#9111 = AXIS2_PLACEMENT_3D ( 'NONE', #12863, #9433, #9511 ) ;
#9112 = CARTESIAN_POINT ( 'NONE',  ( 12.07479981346994258, 61.83277384271320187, 17.09860361742227397 ) ) ;
#9113 = DIRECTION ( 'NONE',  ( 1.000000000000000000, 0.000000000000000000, 0.000000000000000000 ) ) ;
#9114 = VERTEX_POINT ( 'NONE', #8364 ) ;
#9115 = LINE ( 'NONE', #3349, #1822 ) ;
#9116 = B_SPLINE_CURVE_WITH_KNOTS ( 'NONE', 3,
 ( #8399, #13108, #2854, #428, #8617, #6026, #578, #7239, #5134, #5210, #14247, #14314, #13036, #8462, #7404, #14475, #9525, #11983, #4077, #13187 ),
 .UNSPECIFIED., .F., .F.,
 ( 4, 2, 2, 2, 2, 2, 2, 2, 2, 4 ),
 ( 0.000000000000000000, 0.0009765910691878001981, 0.001464886603781702466, 0.001953182138375604733, 0.002929773207563409268, 0.003906364276751213803, 0.004882955345939018338, 0.005859546415126822873, 0.006836137484314629142, 0.007812728553502436279 ),
 .UNSPECIFIED. ) ;
#9117 = CARTESIAN_POINT ( 'NONE',  ( 34.44830544488820578, 94.94374256356070418, 16.00000000000000000 ) ) ;
#9118 = CARTESIAN_POINT ( 'NONE',  ( 0.2790467552932288098, 97.41488903138106537, 10.49999999999999822 ) ) ;
#9119 = DIRECTION ( 'NONE',  ( 1.000000000000000000, 0.000000000000000000, 0.000000000000000000 ) ) ;
#9120 = DIRECTION ( 'NONE',  ( 0.000000000000000000, 0.000000000000000000, -1.000000000000000000 ) ) ;
#9121 = DIRECTION ( 'NONE',  ( 1.000000000000000000, 0.000000000000000000, 0.000000000000000000 ) ) ;
#9122 = CIRCLE ( 'NONE', #638, 4.999999999999995559 ) ;
#9123 = EDGE_CURVE ( 'NONE', #1207, #7348, #14323, .T. ) ;
#9124 = CARTESIAN_POINT ( 'NONE',  ( 90.10640870805727332, 37.02125851216391794, -13.00000000000000178 ) ) ;
#9125 = EDGE_CURVE ( 'NONE', #7240, #14819, #10491, .T. ) ;
#9126 = EDGE_CURVE ( 'NONE', #1282, #2937, #7772, .T. ) ;
#9127 = EDGE_CURVE ( 'NONE', #11326, #212, #2722, .T. ) ;
#9128 =( LENGTH_UNIT ( ) NAMED_UNIT ( * ) SI_UNIT ( .MILLI., .METRE. ) );
#9129 = ORIENTED_EDGE ( 'NONE', *, *, #13875, .F. ) ;
#9130 = CARTESIAN_POINT ( 'NONE',  ( -68.58935777509570642, -68.58935777509452691, -13.00000000000000178 ) ) ;
#9131 = DIRECTION ( 'NONE',  ( 0.000000000000000000, 0.000000000000000000, 1.000000000000000000 ) ) ;
#9132 = DIRECTION ( 'NONE',  ( 1.000000000000000000, 0.000000000000000000, 0.000000000000000000 ) ) ;
#9133 = PRODUCT_DEFINITION_SHAPE ( 'NONE', 'NONE',  #15040 ) ;
#9134 = PLANE ( 'NONE',  #14397 ) ;
#9135 = ORIENTED_EDGE ( 'NONE', *, *, #6242, .F. ) ;
#9136 = CARTESIAN_POINT ( 'NONE',  ( 54.99999999999999289, 2.055000000000001492, 0.000000000000000000 ) ) ;
#9137 = ORIENTED_EDGE ( 'NONE', *, *, #9029, .F. ) ;
#9138 = EDGE_CURVE ( 'NONE', #6594, #9373, #1960, .T. ) ;
#9139 = CYLINDRICAL_SURFACE ( 'NONE', #1939, 63.00000000000000000 ) ;
#9140 = CARTESIAN_POINT ( 'NONE',  ( -25.00000000000000000, 81.24038404635962252, -23.50000000000000000 ) ) ;
#9141 = DIRECTION ( 'NONE',  ( -1.000000000000000000, 0.000000000000000000, 0.000000000000000000 ) ) ;
#9142 = CARTESIAN_POINT ( 'NONE',  ( 0.000000000000000000, 4.618802153517009401, -3.433295621305381573 ) ) ;
#9143 = ORIENTED_EDGE ( 'NONE', *, *, #13225, .T. ) ;
#9144 = EDGE_CURVE ( 'NONE', #9553, #2051, #256, .T. ) ;
#9145 = EDGE_LOOP ( 'NONE', ( #3029, #12447, #14622, #4252, #9781 ) ) ;
#9146 = ORIENTED_EDGE ( 'NONE', *, *, #12247, .T. ) ;
#9147 = ORIENTED_EDGE ( 'NONE', *, *, #11364, .F. ) ;
#9148 = DIRECTION ( 'NONE',  ( 0.000000000000000000, 0.000000000000000000, 1.000000000000000000 ) ) ;
#9149 = CARTESIAN_POINT ( 'NONE',  ( 32.45630819848047111, 101.9391205390361250, 14.06872601623944696 ) ) ;
#9150 = LINE ( 'NONE', #3544, #9017 ) ;
#9151 = VERTEX_POINT ( 'NONE', #13291 ) ;
#9152 = VERTEX_POINT ( 'NONE', #2744 ) ;
#9153 = ORIENTED_EDGE ( 'NONE', *, *, #2949, .T. ) ;
#9154 = CARTESIAN_POINT ( 'NONE',  ( -12.86891638962156215, 56.43380494353993271, -8.000000000000000000 ) ) ;
#9155 = CYLINDRICAL_SURFACE ( 'NONE', #14589, 0.5000000000000004441 ) ;
#9156 = CARTESIAN_POINT ( 'NONE',  ( -13.71740939043329277, 51.19406879332069593, -10.50000000000000000 ) ) ;
#9157 =( NAMED_UNIT ( * ) PLANE_ANGLE_UNIT ( ) SI_UNIT ( $, .RADIAN. ) );
#9158 = DIRECTION ( 'NONE',  ( 1.000000000000000000, 0.000000000000000000, 0.000000000000000000 ) ) ;
#9159 = VERTEX_POINT ( 'NONE', #8576 ) ;
#9160 = PLANE ( 'NONE',  #11923 ) ;
#9161 = ORIENTED_EDGE ( 'NONE', *, *, #5815, .F. ) ;
#9162 = DIRECTION ( 'NONE',  ( 0.000000000000000000, 0.000000000000000000, 1.000000000000000000 ) ) ;
#9164 = EDGE_CURVE ( 'NONE', #10988, #11670, #7438, .T. ) ;
#9163 = ORIENTED_EDGE ( 'NONE', *, *, #11280, .T. ) ;
#9165 = AXIS2_PLACEMENT_3D ( 'NONE', #135, #200, #10830 ) ;
#9166 = ADVANCED_FACE ( 'NONE', ( #11015 ), #12086, .F. ) ;
#9167 = ORIENTED_EDGE ( 'NONE', *, *, #5724, .F. ) ;
#9168 = ADVANCED_FACE ( 'NONE', ( #1455 ), #14354, .T. ) ;
#9169 = ADVANCED_FACE ( 'NONE', ( #317 ), #6285, .F. ) ;
#9170 = ORIENTED_EDGE ( 'NONE', *, *, #6043, .T. ) ;
#9171 = MANIFOLD_SOLID_BREP ( 'Boss-Extrude1', #5990 ) ;
#9172 = FACE_OUTER_BOUND ( 'NONE', #10700, .T. ) ;
#9173 = EDGE_CURVE ( 'NONE', #8983, #5358, #13150, .T. ) ;
#9174 = DIRECTION ( 'NONE',  ( -0.000000000000000000, -0.000000000000000000, -1.000000000000000000 ) ) ;
#9175 = DIRECTION ( 'NONE',  ( -0.000000000000000000, -0.000000000000000000, 1.000000000000000000 ) ) ;
#9176 = CARTESIAN_POINT ( 'NONE',  ( 0.1750025118121574796, 4.719839900820618439, -3.469254087858248514 ) ) ;
#9177 = ORIENTED_EDGE ( 'NONE', *, *, #1846, .T. ) ;
#9178 = LINE ( 'NONE', #8118, #5318 ) ;
#9179 = EDGE_LOOP ( 'NONE', ( #4736, #12753, #7721, #7231 ) ) ;
#9180 = FILL_AREA_STYLE_COLOUR ( '', #4147 ) ;
#9181 = EDGE_CURVE ( 'NONE', #10382, #11572, #10937, .T. ) ;
#9182 = DIRECTION ( 'NONE',  ( 0.000000000000000000, 0.000000000000000000, 1.000000000000000000 ) ) ;
#9183 = ORIENTED_EDGE ( 'NONE', *, *, #13997, .T. ) ;
#9184 = FACE_OUTER_BOUND ( 'NONE', #12887, .T. ) ;
#9185 = VECTOR ( 'NONE', #10096, 1000.000000000000000 ) ;
#9186 = DIRECTION ( 'NONE',  ( -1.000000000000000000, 0.000000000000000000, 0.000000000000000000 ) ) ;
#9187 = CARTESIAN_POINT ( 'NONE',  ( -10.19763225997207101, 62.16969414240132608, 19.21937000502254023 ) ) ;
#9188 = CARTESIAN_POINT ( 'NONE',  ( -2.449293598294708880E-16, 38.00000000000000000, -25.50000000000000355 ) ) ;
#9189 = CARTESIAN_POINT ( 'NONE',  ( 42.04772703543530099, 32.26435573746242369, -8.000000000000000000 ) ) ;
#9190 = LINE ( 'NONE', #9, #4383 ) ;
#9191 = AXIS2_PLACEMENT_3D ( 'NONE', #9377, #8238, #14025 ) ;
#9192 = FACE_OUTER_BOUND ( 'NONE', #12656, .T. ) ;
#9193 = AXIS2_PLACEMENT_3D ( 'NONE', #2415, #6737, #1293 ) ;
#9194 = DIRECTION ( 'NONE',  ( 0.8191520442889902442, 1.003171929053522651E-16, -0.5735764363510482688 ) ) ;
#9195 = ORIENTED_EDGE ( 'NONE', *, *, #12989, .F. ) ;
#9196 = DIRECTION ( 'NONE',  ( -0.000000000000000000, -0.000000000000000000, 1.000000000000000000 ) ) ;
#9197 = DIRECTION ( 'NONE',  ( 1.000000000000000000, 0.000000000000000000, 0.000000000000000000 ) ) ;
#9198 = CARTESIAN_POINT ( 'NONE',  ( 89.61631465359468507, -37.12029293941410657, -13.00000000000000178 ) ) ;
#9199 = ORIENTED_EDGE ( 'NONE', *, *, #8056, .T. ) ;
#9200 = CIRCLE ( 'NONE', #8959, 2.649999999999985700 ) ;
#9201 = DIRECTION ( 'NONE',  ( -0.000000000000000000, -0.000000000000000000, 1.000000000000000000 ) ) ;
#9202 = EDGE_LOOP ( 'NONE', ( #5324, #7478, #9618, #12990 ) ) ;
#9203 = CIRCLE ( 'NONE', #11157, 100.0000000000000000 ) ;
#9204 = EDGE_CURVE ( 'NONE', #5057, #13764, #4956, .T. ) ;
#9205 = CARTESIAN_POINT ( 'NONE',  ( -1.674280531759324342, -99.48933418828643482, 8.000000000000000000 ) ) ;
#9206 = CIRCLE ( 'NONE', #8721, 56.99999999999999289 ) ;
#9207 = EDGE_CURVE ( 'NONE', #14795, #10139, #8650, .T. ) ;
#9208 = ORIENTED_EDGE ( 'NONE', *, *, #10712, .F. ) ;
#9209 = AXIS2_PLACEMENT_3D ( 'NONE', #11412, #10266, #14907 ) ;
#9210 = FACE_OUTER_BOUND ( 'NONE', #140, .T. ) ;
#9211 = DIRECTION ( 'NONE',  ( 0.000000000000000000, 0.000000000000000000, 1.000000000000000000 ) ) ;
#9212 = DIRECTION ( 'NONE',  ( 1.000000000000000000, 0.000000000000000000, 0.000000000000000000 ) ) ;
#9213 = CARTESIAN_POINT ( 'NONE',  ( -25.00000000000000000, 81.24038404635962252, -31.00000000000000000 ) ) ;
#9214 = ORIENTED_EDGE ( 'NONE', *, *, #14952, .T. ) ;
#9215 = ORIENTED_EDGE ( 'NONE', *, *, #595, .F. ) ;
#9216 = AXIS2_PLACEMENT_3D ( 'NONE', #2687, #7302, #11959 ) ;
#9217 = CARTESIAN_POINT ( 'NONE',  ( -12.39897948556635754, 61.76783392443436327, -16.00000000000000000 ) ) ;
#9218 = CIRCLE ( 'NONE', #11167, 3.000000000000002665 ) ;
#9219 = CARTESIAN_POINT ( 'NONE',  ( -33.48561063518626923, 47.21331623427104063, -8.000000000000000000 ) ) ;
#9220 = AXIS2_PLACEMENT_3D ( 'NONE', #13665, #7890, #2123 ) ;
#9221 = PRODUCT_RELATED_PRODUCT_CATEGORY ( 'part', '', ( #5123 ) ) ;
#9222 = DIRECTION ( 'NONE',  ( -1.000000000000000000, 0.000000000000000000, 0.000000000000000000 ) ) ;
#9223 = ORIENTED_EDGE ( 'NONE', *, *, #416, .T. ) ;
#9224 = EDGE_LOOP ( 'NONE', ( #1653, #6729, #7102, #11182 ) ) ;
#9225 = ADVANCED_FACE ( 'NONE', ( #8949 ), #13587, .T. ) ;
#9226 = EDGE_CURVE ( 'NONE', #11082, #5022, #2196, .T. ) ;
#9227 = VECTOR ( 'NONE', #997, 1000.000000000000000 ) ;
#9228 = ORIENTED_EDGE ( 'NONE', *, *, #1585, .F. ) ;
#9229 = AXIS2_PLACEMENT_3D ( 'NONE', #11768, #2801, #9680 ) ;
#9230 = DIRECTION ( 'NONE',  ( -1.000000000000000000, 0.000000000000000000, 0.000000000000000000 ) ) ;
#9231 = AXIS2_PLACEMENT_3D ( 'NONE', #8236, #6024, #13882 ) ;
#9232 = CARTESIAN_POINT ( 'NONE',  ( -2.059999999999998721, 2.522772406243545965E-16, -0.3080913168122742518 ) ) ;
#9233 = VECTOR ( 'NONE', #2946, 1000.000000000000000 ) ;
#9234 = DIRECTION ( 'NONE',  ( 1.000000000000000000, 8.881784197001252323E-16, 0.000000000000000000 ) ) ;
#9235 = CYLINDRICAL_SURFACE ( 'NONE', #4029, 3.000000000000002665 ) ;
#9236 = CARTESIAN_POINT ( 'NONE',  ( 56.43380494353997534, 12.86891638962136319, -10.50000000000000000 ) ) ;
#9237 = ORIENTED_EDGE ( 'NONE', *, *, #8474, .F. ) ;
#9238 = ORIENTED_EDGE ( 'NONE', *, *, #11571, .F. ) ;
#9239 = DIRECTION ( 'NONE',  ( 1.000000000000000000, 0.000000000000000000, 0.000000000000000000 ) ) ;
#9240 = DIRECTION ( 'NONE',  ( 0.000000000000000000, 0.000000000000000000, 1.000000000000000000 ) ) ;
#9241 = CIRCLE ( 'NONE', #3919, 95.00000000000001421 ) ;
#9242 = ORIENTED_EDGE ( 'NONE', *, *, #9204, .F. ) ;
#9243 = CIRCLE ( 'NONE', #3922, 2.649999999999992806 ) ;
#9244 = CIRCLE ( 'NONE', #770, 0.5000000000000038858 ) ;
#9245 = ORIENTED_EDGE ( 'NONE', *, *, #1702, .T. ) ;
#9246 = DIRECTION ( 'NONE',  ( 1.000000000000000000, 0.000000000000000000, 0.000000000000000000 ) ) ;
#9247 = ORIENTED_EDGE ( 'NONE', *, *, #172, .T. ) ;
#9248 = DIRECTION ( 'NONE',  ( 0.000000000000000000, 0.000000000000000000, 1.000000000000000000 ) ) ;
#9249 = DIRECTION ( 'NONE',  ( 0.000000000000000000, 0.000000000000000000, -1.000000000000000000 ) ) ;
#9250 = ADVANCED_FACE ( 'NONE', ( #5398, #8806 ), #5616, .T. ) ;
#9251 = CARTESIAN_POINT ( 'NONE',  ( 70.71067811865489716, 70.71067811865461294, -8.000000000000000000 ) ) ;
#9252 = FACE_OUTER_BOUND ( 'NONE', #449, .T. ) ;
#9253 = CARTESIAN_POINT ( 'NONE',  ( 0.5000000000000045519, -97.00000000000000000, -13.00000000000000178 ) ) ;
#9254 = ADVANCED_FACE ( 'NONE', ( #10251 ), #2054, .T. ) ;
#9255 = ORIENTED_EDGE ( 'NONE', *, *, #9727, .T. ) ;
#9256 = PLANE ( 'NONE',  #4632 ) ;
#9257 = EDGE_CURVE ( 'NONE', #12166, #4396, #787, .T. ) ;
#9258 = CARTESIAN_POINT ( 'NONE',  ( 69.20695371924547601, 57.06275842387054098, 10.49999999999999822 ) ) ;
#9259 = AXIS2_PLACEMENT_3D ( 'NONE', #11247, #1828, #11395 ) ;
#9260 = ORIENTED_EDGE ( 'NONE', *, *, #10328, .T. ) ;
#9261 = CARTESIAN_POINT ( 'NONE',  ( 89.61631465359491244, 37.12029293941346708, -8.000000000000000000 ) ) ;
#9262 = DIRECTION ( 'NONE',  ( -0.000000000000000000, -0.000000000000000000, -1.000000000000000000 ) ) ;
#9263 = AXIS2_PLACEMENT_3D ( 'NONE', #8591, #5038, #2757 ) ;
#9264 = ORIENTED_EDGE ( 'NONE', *, *, #4734, .T. ) ;
#9265 = CARTESIAN_POINT ( 'NONE',  ( -11.08335940112994855, 62.01770010158976731, 18.49860775790518730 ) ) ;
#9266 = EDGE_CURVE ( 'NONE', #7158, #5002, #5113, .T. ) ;
#9267 = ADVANCED_FACE ( 'NONE', ( #14742 ), #2967, .T. ) ;
#9268 = LINE ( 'NONE', #8202, #12737 ) ;
#9269 = CARTESIAN_POINT ( 'NONE',  ( -10.80089892394231832, 106.4537193389066374, 18.76964747820619905 ) ) ;
#9270 = CARTESIAN_POINT ( 'NONE',  ( -27.94117647058823550, 90.79807628710781842, -23.50000000000000000 ) ) ;
#9271 = CARTESIAN_POINT ( 'NONE',  ( 0.000000000000000000, 0.000000000000000000, -26.00000000000000000 ) ) ;
#9272 = PRODUCT_CONTEXT ( 'NONE', #6085, 'mechanical' ) ;
#9273 = CIRCLE ( 'NONE', #1519, 0.5000000000000022204 ) ;
#9274 = CARTESIAN_POINT ( 'NONE',  ( -45.39934640057513349, 26.50000000000019540, 10.49999999999999822 ) ) ;
#9275 = ORIENTED_EDGE ( 'NONE', *, *, #5340, .T. ) ;
#9276 = VECTOR ( 'NONE', #12174, 1000.000000000000000 ) ;
#9277 = DIRECTION ( 'NONE',  ( 0.000000000000000000, 0.000000000000000000, 1.000000000000000000 ) ) ;
#9278 = CARTESIAN_POINT ( 'NONE',  ( 7.500000000000000888, 94.70348462437907244, -20.00000000000000000 ) ) ;
#9279 = CARTESIAN_POINT ( 'NONE',  ( 0.000000000000000000, 0.000000000000000000, 8.000000000000000000 ) ) ;
#9280 = CARTESIAN_POINT ( 'NONE',  ( -52.54657765281192638, 6.917888187662934563, 10.49999999999999822 ) ) ;
#9281 = AXIS2_PLACEMENT_3D ( 'NONE', #4440, #10350, #13852 ) ;
#9282 = ORIENTED_EDGE ( 'NONE', *, *, #7417, .T. ) ;
#9283 = DIRECTION ( 'NONE',  ( 0.000000000000000000, 0.000000000000000000, 1.000000000000000000 ) ) ;
#9284 = EDGE_LOOP ( 'NONE', ( #11139, #13656, #4098, #4317, #14592, #6588, #4548, #5961, #2309, #13887 ) ) ;
#9285 = CYLINDRICAL_SURFACE ( 'NONE', #2551, 22.00000000000000355 ) ;
#9286 = CIRCLE ( 'NONE', #4935, 52.50000000000000711 ) ;
#9287 = DIRECTION ( 'NONE',  ( 1.000000000000000000, 0.000000000000000000, 0.000000000000000000 ) ) ;
#9288 = CARTESIAN_POINT ( 'NONE',  ( -3.999999999999996447, 2.309401076758498039, -3.433295621305378020 ) ) ;
#9289 = VERTEX_POINT ( 'NONE', #12312 ) ;
#9290 = AXIS2_PLACEMENT_3D ( 'NONE', #6484, #14714, #4314 ) ;
#9291 = ORIENTED_EDGE ( 'NONE', *, *, #14471, .F. ) ;
#9292 = CARTESIAN_POINT ( 'NONE',  ( -45.89934640057513349, 26.50000000000019540, -8.000000000000000000 ) ) ;
#9293 = FACE_OUTER_BOUND ( 'NONE', #8044, .T. ) ;
#9294 = CARTESIAN_POINT ( 'NONE',  ( -30.80502811811232888, -49.00442420935981147, -13.00000000000000178 ) ) ;
#9295 = ORIENTED_EDGE ( 'NONE', *, *, #14991, .F. ) ;
#9296 = AXIS2_PLACEMENT_3D ( 'NONE', #6771, #2155, #7995 ) ;
#9297 = VERTEX_POINT ( 'NONE', #8880 ) ;
#9298 = VERTEX_POINT ( 'NONE', #1898 ) ;
#9299 = DIRECTION ( 'NONE',  ( 0.000000000000000000, 0.000000000000000000, -1.000000000000000000 ) ) ;
#9300 = DIRECTION ( 'NONE',  ( -1.000000000000000000, 0.000000000000000000, 0.000000000000000000 ) ) ;
#9301 = CARTESIAN_POINT ( 'NONE',  ( 4.140404888673279160, 2.228338276487440428, -3.686887068327035610 ) ) ;
#9302 = SURFACE_SIDE_STYLE ('',( #3472 ) ) ;
#9303 = CARTESIAN_POINT ( 'NONE',  ( -2.100000000000000089, 2.571758278209443929E-16, -0.2800830152838856835 ) ) ;
#9304 = AXIS2_PLACEMENT_3D ( 'NONE', #12093, #4807, #7742 ) ;
#9305 = CIRCLE ( 'NONE', #99, 5.000000000000001776 ) ;
#9306 = DIRECTION ( 'NONE',  ( 0.000000000000000000, 0.000000000000000000, 1.000000000000000000 ) ) ;
#9307 = EDGE_LOOP ( 'NONE', ( #1710, #12322, #1234, #12991 ) ) ;
#9308 = ADVANCED_FACE ( 'NONE', ( #13670 ), #12460, .F. ) ;
#9309 = ADVANCED_FACE ( 'NONE', ( #4340 ), #6510, .F. ) ;
#9310 = VERTEX_POINT ( 'NONE', #14814 ) ;
#9311 = ADVANCED_FACE ( 'NONE', ( #3195 ), #7812, .F. ) ;
#9312 = DIRECTION ( 'NONE',  ( 0.000000000000000000, 0.000000000000000000, -1.000000000000000000 ) ) ;
#9313 = DIRECTION ( 'NONE',  ( 0.000000000000000000, 0.000000000000000000, 1.000000000000000000 ) ) ;
#9314 = EDGE_CURVE ( 'NONE', #1107, #10590, #10926, .T. ) ;
#9315 = ORIENTED_EDGE ( 'NONE', *, *, #12933, .F. ) ;
#9316 = ORIENTED_EDGE ( 'NONE', *, *, #1067, .F. ) ;
#9317 = DIRECTION ( 'NONE',  ( 0.000000000000000000, 0.000000000000000000, 1.000000000000000000 ) ) ;
#9318 = CIRCLE ( 'NONE', #6391, 3.000000000000002665 ) ;
#9319 = ADVANCED_FACE ( 'NONE', ( #926 ), #5314, .F. ) ;
#9320 = AXIS2_PLACEMENT_3D ( 'NONE', #13032, #8315, #10593 ) ;
#9321 = EDGE_LOOP ( 'NONE', ( #11267, #9896, #7065, #12508, #14955, #13240, #2323, #4465 ) ) ;
#9322 = ORIENTED_EDGE ( 'NONE', *, *, #11684, .F. ) ;
#9323 = DIRECTION ( 'NONE',  ( 0.000000000000000000, 0.000000000000000000, -1.000000000000000000 ) ) ;
#9324 = DIRECTION ( 'NONE',  ( -0.000000000000000000, -0.000000000000000000, -1.000000000000000000 ) ) ;
#9325 = CARTESIAN_POINT ( 'NONE',  ( 25.00000000000000000, 81.24038404635960831, 16.00000000000000000 ) ) ;
#9326 = CARTESIAN_POINT ( 'NONE',  ( 0.000000000000000000, 0.000000000000000000, 8.000000000000000000 ) ) ;
#9327 = CARTESIAN_POINT ( 'NONE',  ( -11.62988759722695953, 74.09296836101485439, -17.83282915334323349 ) ) ;
#9328 = DIRECTION ( 'NONE',  ( 0.000000000000000000, 0.000000000000000000, 1.000000000000000000 ) ) ;
#9329 = ORIENTED_EDGE ( 'NONE', *, *, #1435, .T. ) ;
#9330 = AXIS2_PLACEMENT_3D ( 'NONE', #10889, #2921, #1788 ) ;
#9331 = CIRCLE ( 'NONE', #8121, 17.00000000000000711 ) ;
#9332 = SURFACE_STYLE_USAGE ( .BOTH. , #14045 ) ;
#9333 = AXIS2_PLACEMENT_3D ( 'NONE', #1160, #11493, #2588 ) ;
#9334 = PLANE ( 'NONE',  #14764 ) ;
#9335 = ADVANCED_FACE ( 'NONE', ( #12538, #2128, #693, #9942, #14593, #4193, #3343 ), #9256, .T. ) ;
#9336 = ORIENTED_EDGE ( 'NONE', *, *, #3245, .F. ) ;
#9337 = CARTESIAN_POINT ( 'NONE',  ( 30.80502811811196295, 49.00442420936003174, -10.50000000000000000 ) ) ;
#9338 = CARTESIAN_POINT ( 'NONE',  ( 1.391697335622809728, 4.043246145443373685, -3.503898532754365913 ) ) ;
#9339 = CIRCLE ( 'NONE', #8855, 50.00000000000000000 ) ;
#9340 = CARTESIAN_POINT ( 'NONE',  ( -12.86891638962156215, 56.43380494353993271, -13.00000000000000178 ) ) ;
#9341 = CARTESIAN_POINT ( 'NONE',  ( -94.51066581171356518, -1.674280531758327140, -8.000000000000000000 ) ) ;
#9342 = CARTESIAN_POINT ( 'NONE',  ( 0.000000000000000000, 0.000000000000000000, -8.000000000000000000 ) ) ;
#9343 = MANIFOLD_SOLID_BREP ( 'Hex', #10854 ) ;
#9344 = CARTESIAN_POINT ( 'NONE',  ( -4.211399284164270007, 2.459729995988209073, -3.751162237960540491 ) ) ;
#9345 = ITEM_DEFINED_TRANSFORMATION ( 'NONE', 'NONE', #3379,  #5108 ) ;
#9346 = CIRCLE ( 'NONE', #11052, 53.55662432702593634 ) ;
#9347 = DIRECTION ( 'NONE',  ( 0.000000000000000000, 0.000000000000000000, 1.000000000000000000 ) ) ;
#9348 = CIRCLE ( 'NONE', #5952, 3.000000000000002665 ) ;
#9349 = ORIENTED_EDGE ( 'NONE', *, *, #7794, .F. ) ;
#9350 = CARTESIAN_POINT ( 'NONE',  ( -12.46748823216054625, 106.2711901036691273, -15.65608700630148675 ) ) ;
#9351 = CARTESIAN_POINT ( 'NONE',  ( 8.636355552181207429, 94.60704768011227372, -19.87755835258713688 ) ) ;
#9352 = EDGE_CURVE ( 'NONE', #5870, #6495, #5831, .T. ) ;
#9353 = EDGE_CURVE ( 'NONE', #4977, #8921, #1215, .T. ) ;
#9354 = CARTESIAN_POINT ( 'NONE',  ( -39.30189486418265687, -33.47282819776598473, 8.000000000000000000 ) ) ;
#9355 = LINE ( 'NONE', #1027, #5910 ) ;
#9356 = ORIENTED_EDGE ( 'NONE', *, *, #1299, .T. ) ;
#9357 = AXIS2_PLACEMENT_3D ( 'NONE', #2765, #7387, #9651 ) ;
#9358 = LINE ( 'NONE', #2235, #7295 ) ;
#9359 = ORIENTED_EDGE ( 'NONE', *, *, #2351, .T. ) ;
#9360 = CARTESIAN_POINT ( 'NONE',  ( -3.680118525130241736, 2.494084732383326841, -0.3507732604232432494 ) ) ;
#9361 = DIRECTION ( 'NONE',  ( 1.000000000000000000, 0.000000000000000000, 0.000000000000000000 ) ) ;
#9362 = EDGE_CURVE ( 'NONE', #10605, #7502, #14584, .T. ) ;
#9363 = DIRECTION ( 'NONE',  ( -0.000000000000000000, -0.000000000000000000, -1.000000000000000000 ) ) ;
#9364 = CYLINDRICAL_SURFACE ( 'NONE', #9296, 60.50000000000000000 ) ;
#9365 = ORIENTED_EDGE ( 'NONE', *, *, #9820, .F. ) ;
#9366 = AXIS2_PLACEMENT_3D ( 'NONE', #6154, #3592, #10795 ) ;
#9367 = DIRECTION ( 'NONE',  ( 1.000000000000000000, 0.000000000000000000, 0.000000000000000000 ) ) ;
#9368 = DIRECTION ( 'NONE',  ( -1.000000000000000000, 0.000000000000000000, 0.000000000000000000 ) ) ;
#9369 = ADVANCED_FACE ( 'NONE', ( #3499 ), #10475, .F. ) ;
#9370 = DIRECTION ( 'NONE',  ( -1.000000000000000000, 0.000000000000000000, 0.000000000000000000 ) ) ;
#9371 = ORIENTED_EDGE ( 'NONE', *, *, #12727, .F. ) ;
#9372 = ORIENTED_EDGE ( 'NONE', *, *, #11745, .F. ) ;
#9373 = VERTEX_POINT ( 'NONE', #8122 ) ;
#9374 = DIRECTION ( 'NONE',  ( 1.000000000000000000, 0.000000000000000000, 0.000000000000000000 ) ) ;
#9375 = LINE ( 'NONE', #47, #6553 ) ;
#9376 = CARTESIAN_POINT ( 'NONE',  ( 1.274258131565028318, 3.883108878240871586, -3.220599429844048789 ) ) ;
#9377 = CARTESIAN_POINT ( 'NONE',  ( 0.000000000000000000, 0.000000000000000000, 0.000000000000000000 ) ) ;
#9378 = FACE_OUTER_BOUND ( 'NONE', #5562, .T. ) ;
#9379 = CARTESIAN_POINT ( 'NONE',  ( 97.00000000000000000, -3.384287605079545030E-13, 10.49999999999999822 ) ) ;
#9380 = ORIENTED_EDGE ( 'NONE', *, *, #6528, .F. ) ;
#9381 = ORIENTED_EDGE ( 'NONE', *, *, #4912, .F. ) ;
#9382 = CARTESIAN_POINT ( 'NONE',  ( -45.89934640057513349, 26.50000000000019540, 10.49999999999999822 ) ) ;
#9383 = DIRECTION ( 'NONE',  ( 0.000000000000000000, 0.000000000000000000, 1.000000000000000000 ) ) ;
#9384 = DIRECTION ( 'NONE',  ( 0.000000000000000000, 0.000000000000000000, -1.000000000000000000 ) ) ;
#9385 = ORIENTED_EDGE ( 'NONE', *, *, #3311, .F. ) ;
#9386 = VERTEX_POINT ( 'NONE', #2283 ) ;
#9387 = CARTESIAN_POINT ( 'NONE',  ( -37.71449950290985953, 86.67575032682117353, 8.000000000000000000 ) ) ;
#9388 = VERTEX_POINT ( 'NONE', #71 ) ;
#9389 = EDGE_CURVE ( 'NONE', #1392, #11614, #8745, .T. ) ;
#9390 = CARTESIAN_POINT ( 'NONE',  ( -19.99999999999998934, 64.99230723708770086, -26.00000000000000000 ) ) ;
#9391 = FACE_OUTER_BOUND ( 'NONE', #14732, .T. ) ;
#9392 = EDGE_CURVE ( 'NONE', #900, #1607, #9469, .T. ) ;
#9393 = DIRECTION ( 'NONE',  ( 1.000000000000000000, 0.000000000000000000, 0.000000000000000000 ) ) ;
#9394 = VERTEX_POINT ( 'NONE', #11562 ) ;
#9395 = DIRECTION ( 'NONE',  ( 0.2941176470588241498, -0.9557692240748186796, 0.000000000000000000 ) ) ;
#9396 = AXIS2_PLACEMENT_3D ( 'NONE', #2633, #14031, #1356 ) ;
#9397 = CARTESIAN_POINT ( 'NONE',  ( 0.000000000000000000, 0.000000000000000000, 8.000000000000000000 ) ) ;
#9398 = ORIENTED_EDGE ( 'NONE', *, *, #12481, .T. ) ;
#9399 =( NAMED_UNIT ( * ) SI_UNIT ( $, .STERADIAN. ) SOLID_ANGLE_UNIT ( ) );
#9400 = ORIENTED_EDGE ( 'NONE', *, *, #5634, .F. ) ;
#9401 = CARTESIAN_POINT ( 'NONE',  ( -53.20607447915234189, 6.117650515114558374, -10.50000000000000000 ) ) ;
#9402 = ORIENTED_EDGE ( 'NONE', *, *, #6565, .T. ) ;
#9403 = CARTESIAN_POINT ( 'NONE',  ( -68.58935777509427112, 68.58935777509594800, -13.00000000000000178 ) ) ;
#9404 = ORIENTED_EDGE ( 'NONE', *, *, #1928, .F. ) ;
#9405 = EDGE_CURVE ( 'NONE', #8537, #12171, #2208, .T. ) ;
#9406 = DIRECTION ( 'NONE',  ( -1.000000000000000000, 0.000000000000000000, 0.000000000000000000 ) ) ;
#9407 = DIRECTION ( 'NONE',  ( 0.000000000000000000, 0.000000000000000000, 1.000000000000000000 ) ) ;
#9408 = CARTESIAN_POINT ( 'NONE',  ( -10.00086283267471465, 106.5319533799504939, 19.34189422912923817 ) ) ;
#9409 = CARTESIAN_POINT ( 'NONE',  ( 5.384454397937118664, 0.000000000000000000, -5.000000000000000888 ) ) ;
#9410 = AXIS2_PLACEMENT_3D ( 'NONE', #9006, #12515, #8861 ) ;
#9411 = CARTESIAN_POINT ( 'NONE',  ( 25.00000000000000000, 81.24038404635960831, 13.50000000000000533 ) ) ;
#9412 = APPLICATION_PROTOCOL_DEFINITION ( 'draft international standard', 'automotive_design', 1998, #5236 ) ;
#9413 = DIRECTION ( 'NONE',  ( 0.000000000000000000, 0.000000000000000000, 1.000000000000000000 ) ) ;
#9414 = ORIENTED_EDGE ( 'NONE', *, *, #4537, .F. ) ;
#9415 = CARTESIAN_POINT ( 'NONE',  ( 1.654252653721904442, 3.663718938583012896, -0.01223254789873389446 ) ) ;
#9416 = CARTESIAN_POINT ( 'NONE',  ( -3.999999999999996447, -2.309401076758518911, -0.5000000000000004441 ) ) ;
#9417 = CARTESIAN_POINT ( 'NONE',  ( 3.999999999999998224, 1.539600717838995658, -3.300726591567077151 ) ) ;
#9418 = CARTESIAN_POINT ( 'NONE',  ( -29.49928053175900899, -45.83364790889059037, 8.000000000000000000 ) ) ;
#9419 = ORIENTED_EDGE ( 'NONE', *, *, #10804, .T. ) ;
#9420 = DIRECTION ( 'NONE',  ( 1.000000000000000000, 0.000000000000000000, 0.000000000000000000 ) ) ;
#9421 = ORIENTED_EDGE ( 'NONE', *, *, #9181, .T. ) ;
#9422 = ORIENTED_EDGE ( 'NONE', *, *, #14136, .F. ) ;
#9423 = DIRECTION ( 'NONE',  ( -1.000000000000000000, 5.335368001743792930E-15, 0.000000000000000000 ) ) ;
#9424 = FACE_OUTER_BOUND ( 'NONE', #8920, .T. ) ;
#9425 = EDGE_CURVE ( 'NONE', #13753, #5547, #3133, .T. ) ;
#9426 = CIRCLE ( 'NONE', #4835, 2.649999999999985700 ) ;
#9427 = EDGE_CURVE ( 'NONE', #9900, #12050, #1077, .T. ) ;
#9428 = DIRECTION ( 'NONE',  ( 1.000000000000000000, 0.000000000000000000, 0.000000000000000000 ) ) ;
#9429 = EDGE_CURVE ( 'NONE', #5812, #14878, #7962, .T. ) ;
#9430 = CARTESIAN_POINT ( 'NONE',  ( 22.33583958711425055, -30.74264578624780597, -28.00000000000000000 ) ) ;
#9431 = EDGE_CURVE ( 'NONE', #2014, #10761, #5691, .T. ) ;
#9432 = ORIENTED_EDGE ( 'NONE', *, *, #2354, .T. ) ;
#9433 = DIRECTION ( 'NONE',  ( 0.000000000000000000, 0.000000000000000000, 1.000000000000000000 ) ) ;
#9434 = DIRECTION ( 'NONE',  ( 0.000000000000000000, 0.000000000000000000, 1.000000000000000000 ) ) ;
#9435 = DIRECTION ( 'NONE',  ( -1.000000000000000000, 0.000000000000000000, 0.000000000000000000 ) ) ;
#9436 = ORIENTED_EDGE ( 'NONE', *, *, #8159, .F. ) ;
#9437 = EDGE_CURVE ( 'NONE', #13133, #13337, #6801, .T. ) ;
#9438 = TOROIDAL_SURFACE ( 'NONE', #3383, 17.00000000000001066, 5.000000000000000000 ) ;
#9439 = CIRCLE ( 'NONE', #12610, 53.55662432702593634 ) ;
#9440 = ORIENTED_EDGE ( 'NONE', *, *, #1664, .T. ) ;
#9441 = VERTEX_POINT ( 'NONE', #7426 ) ;
#9442 = CARTESIAN_POINT ( 'NONE',  ( 12.50000000000000000, 106.2673515243510991, 15.00000000000000000 ) ) ;
#9443 = AXIS2_PLACEMENT_3D ( 'NONE', #1545, #7297, #8444 ) ;
#9444 = DIRECTION ( 'NONE',  ( -1.000000000000000000, 0.000000000000000000, 0.000000000000000000 ) ) ;
#9445 = ADVANCED_FACE ( 'NONE', ( #3869 ), #301, .T. ) ;
#9446 = CARTESIAN_POINT ( 'NONE',  ( 3.999999999999996447, -2.309401076758518911, -3.433295621305385126 ) ) ;
#9447 = FILL_AREA_STYLE ('',( #13035 ) ) ;
#9448 = CIRCLE ( 'NONE', #6525, 95.00000000000001421 ) ;
#9449 = FACE_OUTER_BOUND ( 'NONE', #14682, .T. ) ;
#9450 = CIRCLE ( 'NONE', #1703, 0.5000000000000004441 ) ;
#9451 = ORIENTED_EDGE ( 'NONE', *, *, #7268, .T. ) ;
#9452 = AXIS2_PLACEMENT_3D ( 'NONE', #14192, #12000, #4780 ) ;
#9453 = VERTEX_POINT ( 'NONE', #7345 ) ;
#9454 = CARTESIAN_POINT ( 'NONE',  ( -97.00000000000000000, 1.015776140243522349E-12, -8.000000000000000000 ) ) ;
#9455 = CARTESIAN_POINT ( 'NONE',  ( -68.09867107463028901, -68.49330278050098286, 10.49999999999999822 ) ) ;
#9456 = CARTESIAN_POINT ( 'NONE',  ( 37.62029293941316155, -89.61631465359504034, 10.49999999999999822 ) ) ;
#9457 = ORIENTED_EDGE ( 'NONE', *, *, #1273, .F. ) ;
#9458 = AXIS2_PLACEMENT_3D ( 'NONE', #3510, #6976, #11633 ) ;
#9459 = ORIENTED_EDGE ( 'NONE', *, *, #4957, .F. ) ;
#9460 = CARTESIAN_POINT ( 'NONE',  ( -45.89934640057513349, 26.50000000000019540, -8.000000000000000000 ) ) ;
#9461 = CIRCLE ( 'NONE', #13109, 0.5000000000000038858 ) ;
#9462 = ORIENTED_EDGE ( 'NONE', *, *, #13646, .T. ) ;
#9463 = CIRCLE ( 'NONE', #2931, 50.00000000000000000 ) ;
#9464 = AXIS2_PLACEMENT_3D ( 'NONE', #6047, #7262, #7423 ) ;
#9465 = CARTESIAN_POINT ( 'NONE',  ( -42.50536573064432133, -32.06294366074479996, -13.00000000000000178 ) ) ;
#9466 = DIRECTION ( 'NONE',  ( 0.000000000000000000, 0.000000000000000000, 1.000000000000000000 ) ) ;
#9467 = LINE ( 'NONE', #4171, #5441 ) ;
#9468 = CARTESIAN_POINT ( 'NONE',  ( 0.000000000000000000, 0.000000000000000000, 20.00000000000000000 ) ) ;
#9469 = CIRCLE ( 'NONE', #12638, 2.649999999999987477 ) ;
#9471 = VECTOR ( 'NONE', #2192, 1000.000000000000000 ) ;
#9470 = CARTESIAN_POINT ( 'NONE',  ( -12.26010588040893978, 73.99122283359872654, -16.55683232866783783 ) ) ;
#9472 = CARTESIAN_POINT ( 'NONE',  ( -91.27544013909712817, 39.61975340586647576, -8.000000000000000000 ) ) ;
#9473 = ORIENTED_EDGE ( 'NONE', *, *, #9389, .T. ) ;
#9474 = CIRCLE ( 'NONE', #4403, 100.0000000000000000 ) ;
#9475 = DIRECTION ( 'NONE',  ( -1.000000000000000000, 0.000000000000000000, 0.000000000000000000 ) ) ;
#9476 = AXIS2_PLACEMENT_3D ( 'NONE', #12110, #3917, #2996 ) ;
#9477 = EDGE_CURVE ( 'NONE', #10382, #6653, #12152, .T. ) ;
#9478 = ORIENTED_EDGE ( 'NONE', *, *, #10150, .T. ) ;
#9479 = VERTEX_POINT ( 'NONE', #5075 ) ;
#9480 = CIRCLE ( 'NONE', #11688, 0.5000000000000004441 ) ;
#9481 = DIRECTION ( 'NONE',  ( -1.000000000000000000, 0.000000000000000000, 0.000000000000000000 ) ) ;
#9482 = CARTESIAN_POINT ( 'NONE',  ( 31.47058823529413374, 102.2673069760056563, 31.00000000000000000 ) ) ;
#9483 = FACE_OUTER_BOUND ( 'NONE', #1290, .T. ) ;
#9484 = CARTESIAN_POINT ( 'NONE',  ( -51.79945067148133120, -13.60620885621556475, -10.50000000000000000 ) ) ;
#9485 = CARTESIAN_POINT ( 'NONE',  ( 12.50000000000000000, 100.2235002382176248, -15.00000000000000000 ) ) ;
#9486 = CARTESIAN_POINT ( 'NONE',  ( -57.06275842387042729, 9.706953719246069312, -10.50000000000000000 ) ) ;
#9487 = ITEM_DEFINED_TRANSFORMATION ( 'NONE', 'NONE', #11637,  #5108 ) ;
#9488 = ORIENTED_EDGE ( 'NONE', *, *, #11323, .F. ) ;
#9489 = DIRECTION ( 'NONE',  ( 1.000000000000000000, 0.000000000000000000, -0.000000000000000000 ) ) ;
#9490 = AXIS2_PLACEMENT_3D ( 'NONE', #11190, #11266, #8823 ) ;
#9491 = VERTEX_POINT ( 'NONE', #12005 ) ;
#9492 = ADVANCED_FACE ( 'NONE', ( #1440 ), #8560, .F. ) ;
#9493 = EDGE_CURVE ( 'NONE', #1639, #2908, #3666, .T. ) ;
#9494 = ADVANCED_FACE ( 'NONE', ( #5015 ), #5158, .F. ) ;
#9495 = DIRECTION ( 'NONE',  ( 0.000000000000000000, 0.000000000000000000, 1.000000000000000000 ) ) ;
#9496 = DIRECTION ( 'NONE',  ( 0.000000000000000000, 0.000000000000000000, -1.000000000000000000 ) ) ;
#9497 = CIRCLE ( 'NONE', #8767, 3.000000000000002665 ) ;
#9498 = DIRECTION ( 'NONE',  ( 0.000000000000000000, 0.000000000000000000, 1.000000000000000000 ) ) ;
#9499 = DIRECTION ( 'NONE',  ( 0.000000000000000000, 0.000000000000000000, 1.000000000000000000 ) ) ;
#9500 = ORIENTED_EDGE ( 'NONE', *, *, #11221, .T. ) ;
#9501 = ORIENTED_EDGE ( 'NONE', *, *, #7365, .F. ) ;
#9502 = DIRECTION ( 'NONE',  ( 0.000000000000000000, 0.000000000000000000, 1.000000000000000000 ) ) ;
#9503 = ORIENTED_EDGE ( 'NONE', *, *, #13538, .F. ) ;
#9504 = AXIS2_PLACEMENT_3D ( 'NONE', #4082, #6411, #738 ) ;
#9505 = DIRECTION ( 'NONE',  ( -1.000000000000000000, 0.000000000000000000, 0.000000000000000000 ) ) ;
#9506 = CARTESIAN_POINT ( 'NONE',  ( -19.99999999999998934, 64.99230723708770086, -31.00000000000000000 ) ) ;
#9507 = CARTESIAN_POINT ( 'NONE',  ( 0.000000000000000000, 2.357898499370430834, 0.000000000000000000 ) ) ;
#9508 = CARTESIAN_POINT ( 'NONE',  ( 25.00000000000000000, 81.24038404635960831, -23.50000000000000000 ) ) ;
#9509 = EDGE_LOOP ( 'NONE', ( #10769, #812, #6101, #1901 ) ) ;
#9510 = ORIENTED_EDGE ( 'NONE', *, *, #2114, .T. ) ;
#9511 = DIRECTION ( 'NONE',  ( 1.000000000000000000, 0.000000000000000000, 0.000000000000000000 ) ) ;
#9512 = CARTESIAN_POINT ( 'NONE',  ( -23.49999999999971223, -45.89934640057541060, -13.00000000000000178 ) ) ;
#9513 = AXIS2_PLACEMENT_3D ( 'NONE', #947, #11423, #1024 ) ;
#9514 = CYLINDRICAL_SURFACE ( 'NONE', #7069, 59.49999999999999289 ) ;
#9515 = B_SPLINE_CURVE_WITH_KNOTS ( 'NONE', 3,
 ( #6191, #7247, #9530, #1722 ),
 .UNSPECIFIED., .F., .F.,
 ( 4, 4 ),
 ( 3.469446951953614189E-18, 0.001005167940839970337 ),
 .UNSPECIFIED. ) ;
#9516 = ADVANCED_FACE ( 'NONE', ( #3727 ), #1740, .F. ) ;
#9517 = ORIENTED_EDGE ( 'NONE', *, *, #3287, .T. ) ;
#9518 = AXIS2_PLACEMENT_3D ( 'NONE', #9827, #8768, #12117 ) ;
#9519 = VERTEX_POINT ( 'NONE', #14267 ) ;
#9520 = EDGE_CURVE ( 'NONE', #4822, #10098, #13569, .T. ) ;
#9521 = FACE_OUTER_BOUND ( 'NONE', #11068, .T. ) ;
#9522 = CARTESIAN_POINT ( 'NONE',  ( 8.156204789939931032, 106.6891793314720331, 19.96764982490488904 ) ) ;
#9523 = CARTESIAN_POINT ( 'NONE',  ( 29.49928053175900899, 45.83364790889059037, -13.00000000000000178 ) ) ;
#9524 = FACE_OUTER_BOUND ( 'NONE', #5792, .T. ) ;
#9525 = CARTESIAN_POINT ( 'NONE',  ( -33.22084910410213610, 95.38070844757929478, -15.83879782491089117 ) ) ;
#9526 = ORIENTED_EDGE ( 'NONE', *, *, #14810, .F. ) ;
#9527 = DIRECTION ( 'NONE',  ( -0.000000000000000000, -0.000000000000000000, 1.000000000000000000 ) ) ;
#9528 = CARTESIAN_POINT ( 'NONE',  ( 0.000000000000000000, 0.000000000000000000, 8.000000000000000000 ) ) ;
#9529 = AXIS2_PLACEMENT_3D ( 'NONE', #3458, #12569, #11437 ) ;
#9530 = CARTESIAN_POINT ( 'NONE',  ( 12.46631608856921325, 100.2277185551817809, -15.67011936326128918 ) ) ;
#9531 = EDGE_LOOP ( 'NONE', ( #9947, #8458, #6933, #11818, #433 ) ) ;
#9532 = ADVANCED_FACE ( 'NONE', ( #9689 ), #2729, .F. ) ;
#9533 = EDGE_CURVE ( 'NONE', #3826, #10605, #8477, .T. ) ;
#9534 = VERTEX_POINT ( 'NONE', #10846 ) ;
#9535 = LINE ( 'NONE', #11615, #14452 ) ;
#9536 = ORIENTED_EDGE ( 'NONE', *, *, #485, .T. ) ;
#9537 = AXIS2_PLACEMENT_3D ( 'NONE', #9574, #6004, #1541 ) ;
#9538 = DIRECTION ( 'NONE',  ( 0.000000000000000000, 0.000000000000000000, -1.000000000000000000 ) ) ;
#9539 = MECHANICAL_DESIGN_GEOMETRIC_PRESENTATION_REPRESENTATION (  '', ( #5347 ), #8707 ) ;
#9540 = B_SPLINE_CURVE_WITH_KNOTS ( 'NONE', 3,
 ( #7061, #93, #11504, #4738, #3593, #9416 ),
 .UNSPECIFIED., .F., .F.,
 ( 4, 2, 4 ),
 ( 0.002365888236228000721, 0.003551327329835088017, 0.004736766423442175314 ),
 .UNSPECIFIED. ) ;
#9541 = CARTESIAN_POINT ( 'NONE',  ( 0.000000000000000000, 0.000000000000000000, 8.000000000000000000 ) ) ;
#9542 =( NAMED_UNIT ( * ) SI_UNIT ( $, .STERADIAN. ) SOLID_ANGLE_UNIT ( ) );
#9543 = EDGE_CURVE ( 'NONE', #11817, #4331, #3159, .T. ) ;
#9544 = CYLINDRICAL_SURFACE ( 'NONE', #11183, 95.00000000000001421 ) ;
#9545 = DIRECTION ( 'NONE',  ( -1.000000000000000000, 0.000000000000000000, 0.000000000000000000 ) ) ;
#9546 = ORIENTED_EDGE ( 'NONE', *, *, #7537, .T. ) ;
#9547 = CARTESIAN_POINT ( 'NONE',  ( 7.500000000000000888, 59.24038404635959409, -15.00000000000000355 ) ) ;
#9548 = CIRCLE ( 'NONE', #8587, 0.5000000000000004441 ) ;
#9549 = VECTOR ( 'NONE', #1121, 1000.000000000000000 ) ;
#9550 = VERTEX_POINT ( 'NONE', #14120 ) ;
#9551 = CIRCLE ( 'NONE', #3024, 46.33974596215558961 ) ;
#9552 = EDGE_CURVE ( 'NONE', #11288, #13630, #2650, .T. ) ;
#9553 = VERTEX_POINT ( 'NONE', #8345 ) ;
#9554 = CARTESIAN_POINT ( 'NONE',  ( -12.86891638962156215, 56.43380494353993271, 8.000000000000000000 ) ) ;
#9555 = DIRECTION ( 'NONE',  ( 0.000000000000000000, 0.000000000000000000, 1.000000000000000000 ) ) ;
#9556 = ORIENTED_EDGE ( 'NONE', *, *, #7437, .T. ) ;
#9557 = DIRECTION ( 'NONE',  ( 0.000000000000000000, 0.000000000000000000, -1.000000000000000000 ) ) ;
#9558 = AXIS2_PLACEMENT_3D ( 'NONE', #5500, #11275, #12129 ) ;
#9559 = ORIENTED_EDGE ( 'NONE', *, *, #1131, .F. ) ;
#9560 = CARTESIAN_POINT ( 'NONE',  ( -50.00000000000000000, 0.000000000000000000, -13.00000000000000178 ) ) ;
#9561 = DIRECTION ( 'NONE',  ( -1.000000000000000000, 0.000000000000000000, 0.000000000000000000 ) ) ;
#9562 = DIRECTION ( 'NONE',  ( 1.000000000000000000, 0.000000000000000000, 0.000000000000000000 ) ) ;
#9563 = AXIS2_PLACEMENT_3D ( 'NONE', #13039, #10675, #503 ) ;
#9564 = CIRCLE ( 'NONE', #13701, 60.50000000000000000 ) ;
#9565 = CARTESIAN_POINT ( 'NONE',  ( 36.14014761921570340, 11.74264578624841171, -25.50000000000000355 ) ) ;
#9566 = EDGE_LOOP ( 'NONE', ( #4301, #8759, #11910, #4182, #9163, #6701, #118, #11625, #7445, #10948, #13357, #5490 ) ) ;
#9567 = SURFACE_SIDE_STYLE ('',( #10715 ) ) ;
#9568 = ORIENTED_EDGE ( 'NONE', *, *, #3839, .T. ) ;
#9569 = DIRECTION ( 'NONE',  ( 1.000000000000000000, 0.000000000000000000, 0.000000000000000000 ) ) ;
#9570 = CARTESIAN_POINT ( 'NONE',  ( -57.06275842387042729, 9.706953719246069312, 10.49999999999999822 ) ) ;
#9571 = PRESENTATION_LAYER_ASSIGNMENT (  '', '', ( #117 ) ) ;
#9572 = CARTESIAN_POINT ( 'NONE',  ( 57.06275842387049835, -9.706953719245678514, 8.000000000000000000 ) ) ;
#9573 = CIRCLE ( 'NONE', #1825, 2.041999999999999815 ) ;
#9574 = CARTESIAN_POINT ( 'NONE',  ( 25.00000000000000000, 81.24038404635960831, -13.50000000000000178 ) ) ;
#9575 = ORIENTED_EDGE ( 'NONE', *, *, #14281, .T. ) ;
#9576 = ADVANCED_FACE ( 'NONE', ( #13280 ), #2873, .T. ) ;
#9577 = CARTESIAN_POINT ( 'NONE',  ( 36.14014761921570340, 11.74264578624841171, 14.49999999999999822 ) ) ;
#9578 = ORIENTED_EDGE ( 'NONE', *, *, #10192, .F. ) ;
#9579 = DIRECTION ( 'NONE',  ( 0.9557692240748190127, -0.2941176470588235392, 0.000000000000000000 ) ) ;
#9580 = ADVANCED_FACE ( 'NONE', ( #11849 ), #6051, .F. ) ;
#9581 = FACE_OUTER_BOUND ( 'NONE', #5292, .T. ) ;
#9582 = CIRCLE ( 'NONE', #10566, 55.00000000000000000 ) ;
#9583 = CIRCLE ( 'NONE', #10808, 63.00000000000000000 ) ;
#9584 = CARTESIAN_POINT ( 'NONE',  ( -31.50188236243966244, 102.2577520262375685, -11.65984174646773219 ) ) ;
#9585 = CYLINDRICAL_SURFACE ( 'NONE', #10526, 0.5000000000000004441 ) ;
#9586 = VERTEX_POINT ( 'NONE', #5301 ) ;
#9587 = FACE_OUTER_BOUND ( 'NONE', #1342, .T. ) ;
#9588 = EDGE_CURVE ( 'NONE', #9923, #11548, #4096, .T. ) ;
#9589 = DIRECTION ( 'NONE',  ( 0.000000000000000000, 0.000000000000000000, 1.000000000000000000 ) ) ;
#9590 = CARTESIAN_POINT ( 'NONE',  ( 12.39897948556635754, 100.2360479454198696, -16.00000000000000000 ) ) ;
#9591 = VECTOR ( 'NONE', #12332, 1000.000000000000000 ) ;
#9592 = ORIENTED_EDGE ( 'NONE', *, *, #6060, .F. ) ;
#9593 = PRODUCT_DEFINITION ( 'UNKNOWN', '', #6773, #13177 ) ;
#9594 = DIRECTION ( 'NONE',  ( 0.000000000000000000, 0.000000000000000000, -1.000000000000000000 ) ) ;
#9595 = ORIENTED_EDGE ( 'NONE', *, *, #5791, .F. ) ;
#9596 = DIRECTION ( 'NONE',  ( -0.000000000000000000, -0.000000000000000000, 1.000000000000000000 ) ) ;
#9597 = EDGE_CURVE ( 'NONE', #9719, #8562, #232, .T. ) ;
#9598 = LINE ( 'NONE', #1492, #11973 ) ;
#9599 = DIRECTION ( 'NONE',  ( 0.000000000000000000, 0.000000000000000000, 1.000000000000000000 ) ) ;
#9600 = CARTESIAN_POINT ( 'NONE',  ( 23.50071946824041191, 45.96504489226015977, -8.000000000000000000 ) ) ;
#9601 = AXIS2_PLACEMENT_3D ( 'NONE', #4214, #13247, #11193 ) ;
#9602 = ORIENTED_EDGE ( 'NONE', *, *, #11408, .F. ) ;
#9603 = ORIENTED_EDGE ( 'NONE', *, *, #8898, .T. ) ;
#9604 = CARTESIAN_POINT ( 'NONE',  ( 89.12622059913255157, 37.21932736666302333, -13.00000000000000178 ) ) ;
#9605 = CARTESIAN_POINT ( 'NONE',  ( 52.54657765281197612, -6.917888187662545540, -13.00000000000000178 ) ) ;
#9606 = DIRECTION ( 'NONE',  ( 0.000000000000000000, 0.000000000000000000, -1.000000000000000000 ) ) ;
#9607 = ORIENTED_EDGE ( 'NONE', *, *, #10831, .T. ) ;
#9608 = VERTEX_POINT ( 'NONE', #1961 ) ;
#9609 = PLANE ( 'NONE',  #9835 ) ;
#9610 = ORIENTED_EDGE ( 'NONE', *, *, #8976, .F. ) ;
#9611 = DIRECTION ( 'NONE',  ( 0.000000000000000000, 0.000000000000000000, 1.000000000000000000 ) ) ;
#9612 = DIRECTION ( 'NONE',  ( -1.000000000000000000, 0.000000000000000000, 0.000000000000000000 ) ) ;
#9614 = VERTEX_POINT ( 'NONE', #9924 ) ;
#9613 = EDGE_CURVE ( 'NONE', #4454, #10864, #14799, .T. ) ;
#9615 = DIRECTION ( 'NONE',  ( 0.000000000000000000, 0.000000000000000000, 1.000000000000000000 ) ) ;
#9616 = FACE_OUTER_BOUND ( 'NONE', #13637, .T. ) ;
#9617 = EDGE_CURVE ( 'NONE', #6851, #11617, #8705, .T. ) ;
#9618 = ORIENTED_EDGE ( 'NONE', *, *, #13875, .T. ) ;
#9619 = DIRECTION ( 'NONE',  ( 1.000000000000000000, 0.000000000000000000, 0.000000000000000000 ) ) ;
#9620 = EDGE_CURVE ( 'NONE', #10362, #7077, #1216, .T. ) ;
#9621 = EDGE_LOOP ( 'NONE', ( #8183, #13301, #9627, #12302, #6009 ) ) ;
#9622 = ORIENTED_EDGE ( 'NONE', *, *, #3242, .T. ) ;
#9623 = DIRECTION ( 'NONE',  ( -1.000000000000000000, 0.000000000000000000, 0.000000000000000000 ) ) ;
#9624 = EDGE_CURVE ( 'NONE', #915, #11561, #4120, .T. ) ;
#9625 = ORIENTED_EDGE ( 'NONE', *, *, #12757, .F. ) ;
#9626 = DIRECTION ( 'NONE',  ( 0.000000000000000000, 0.000000000000000000, 1.000000000000000000 ) ) ;
#9627 = ORIENTED_EDGE ( 'NONE', *, *, #13352, .F. ) ;
#9628 = CARTESIAN_POINT ( 'NONE',  ( 22.33583958711425055, -30.74264578624780597, -25.50000000000000355 ) ) ;
#9629 = LINE ( 'NONE', #8644, #11032 ) ;
#9630 = FACE_OUTER_BOUND ( 'NONE', #6632, .T. ) ;
#9631 = CARTESIAN_POINT ( 'NONE',  ( 37.12029293941379393, 89.61631465359479876, 8.000000000000000000 ) ) ;
#9632 = DIRECTION ( 'NONE',  ( -1.000000000000000000, 0.000000000000000000, 0.000000000000000000 ) ) ;
#9633 = ADVANCED_FACE ( 'NONE', ( #10005 ), #1699, .T. ) ;
#9634 = ORIENTED_EDGE ( 'NONE', *, *, #8593, .F. ) ;
#9635 = CARTESIAN_POINT ( 'NONE',  ( 2.500000000000002220, 1.178949249685208533, -2.042000000000002036 ) ) ;
#9636 = ORIENTED_EDGE ( 'NONE', *, *, #2861, .T. ) ;
#9637 = DIRECTION ( 'NONE',  ( 0.000000000000000000, 0.000000000000000000, 1.000000000000000000 ) ) ;
#9638 = DIRECTION ( 'NONE',  ( -1.000000000000000000, 0.000000000000000000, 0.000000000000000000 ) ) ;
#9639 = CARTESIAN_POINT ( 'NONE',  ( -26.99988008862626643, -45.88839665196127271, 10.49999999999999822 ) ) ;
#9640 = DIRECTION ( 'NONE',  ( 1.000000000000000000, 0.000000000000000000, 0.000000000000000000 ) ) ;
#9641 = ORIENTED_EDGE ( 'NONE', *, *, #9759, .F. ) ;
#9642 = CARTESIAN_POINT ( 'NONE',  ( 4.211140560182194292, -2.431303136016555122, -3.745885042887437510 ) ) ;
#9643 = ORIENTED_EDGE ( 'NONE', *, *, #1832, .T. ) ;
#9644 = CYLINDRICAL_SURFACE ( 'NONE', #6529, 20.00000000000000000 ) ;
#9645 = CARTESIAN_POINT ( 'NONE',  ( 4.121772567811984089, 51.45950017607689375, 8.000000000000000000 ) ) ;
#9646 = CARTESIAN_POINT ( 'NONE',  ( -34.65532077583675630, 101.0090414146251447, -15.74457401924681044 ) ) ;
#9647 = CYLINDRICAL_SURFACE ( 'NONE', #8809, 10.00000000000000178 ) ;
#9648 = CARTESIAN_POINT ( 'NONE',  ( 0.000000000000000000, 0.000000000000000000, 16.00000000000000000 ) ) ;
#9649 = ORIENTED_EDGE ( 'NONE', *, *, #7922, .T. ) ;
#9650 = ORIENTED_EDGE ( 'NONE', *, *, #12098, .F. ) ;
#9651 = DIRECTION ( 'NONE',  ( 1.000000000000000000, 0.000000000000000000, 0.000000000000000000 ) ) ;
#9652 = CARTESIAN_POINT ( 'NONE',  ( 33.48561063518626923, -47.21331623427104063, -13.00000000000000178 ) ) ;
#9653 = DIRECTION ( 'NONE',  ( -0.000000000000000000, -0.000000000000000000, 1.000000000000000000 ) ) ;
#9654 = EDGE_CURVE ( 'NONE', #12743, #5953, #10085, .T. ) ;
#9655 = EDGE_CURVE ( 'NONE', #6159, #1593, #3390, .T. ) ;
#9656 = VERTEX_POINT ( 'NONE', #11150 ) ;
#9657 = CARTESIAN_POINT ( 'NONE',  ( 29.70588235294119173, 96.53269163155674448, -10.99999999999999645 ) ) ;
#9658 = CIRCLE ( 'NONE', #10157, 60.50000000000000000 ) ;
#9659 = ORIENTED_EDGE ( 'NONE', *, *, #10242, .F. ) ;
#9660 = DIRECTION ( 'NONE',  ( 1.000000000000000000, 0.000000000000000000, 0.000000000000000000 ) ) ;
#9661 = DIRECTION ( 'NONE',  ( 0.000000000000000000, 0.000000000000000000, -1.000000000000000000 ) ) ;
#9662 = PLANE ( 'NONE',  #9034 ) ;
#9663 = SHAPE_DEFINITION_REPRESENTATION ( #13495, #8006 ) ;
#9664 = CARTESIAN_POINT ( 'NONE',  ( 96.58511096861892042, 0.2790467552928839190, -10.50000000000000000 ) ) ;
#9665 = STYLED_ITEM ( 'NONE', ( #427 ), #6552 ) ;
#9666 = EDGE_LOOP ( 'NONE', ( #4941, #152, #2774, #1932, #2787 ) ) ;
#9667 = LINE ( 'NONE', #9604, #10290 ) ;
#9668 = AXIS2_PLACEMENT_3D ( 'NONE', #2198, #2281, #5761 ) ;
#9669 = CARTESIAN_POINT ( 'NONE',  ( -2.449293598294708880E-16, 38.00000000000000000, 14.49999999999999822 ) ) ;
#9670 = CARTESIAN_POINT ( 'NONE',  ( 42.04772703543530099, 32.26435573746242369, -13.00000000000000178 ) ) ;
#9671 = ADVANCED_FACE ( 'NONE', ( #757 ), #14650, .T. ) ;
#9673 = ORIENTED_EDGE ( 'NONE', *, *, #6012, .F. ) ;
#9672 = EDGE_CURVE ( 'NONE', #2995, #5322, #2790, .T. ) ;
#9674 = ORIENTED_EDGE ( 'NONE', *, *, #593, .F. ) ;
#9675 = CARTESIAN_POINT ( 'NONE',  ( -12.86891638962156215, 56.43380494353993271, -10.50000000000000000 ) ) ;
#9676 = EDGE_CURVE ( 'NONE', #13408, #8680, #14494, .T. ) ;
#9677 = ORIENTED_EDGE ( 'NONE', *, *, #13577, .T. ) ;
#9678 = AXIS2_PLACEMENT_3D ( 'NONE', #9798, #5182, #13083 ) ;
#9679 = AXIS2_PLACEMENT_3D ( 'NONE', #12942, #2533, #7155 ) ;
#9680 = DIRECTION ( 'NONE',  ( -1.000000000000000000, 0.000000000000000000, 0.000000000000000000 ) ) ;
#9681 = CIRCLE ( 'NONE', #7504, 3.000000000000004441 ) ;
#9682 = AXIS2_PLACEMENT_3D ( 'NONE', #10017, #4190, #8943 ) ;
#9683 = DIRECTION ( 'NONE',  ( 0.000000000000000000, 0.000000000000000000, -1.000000000000000000 ) ) ;
#9684 =( LENGTH_UNIT ( ) NAMED_UNIT ( * ) SI_UNIT ( .MILLI., .METRE. ) );
#9685 = ORIENTED_EDGE ( 'NONE', *, *, #8740, .T. ) ;
#9686 = CARTESIAN_POINT ( 'NONE',  ( -44.89637028918153305, 0.000000000000000000, 14.49999999999999822 ) ) ;
#9687 = DIRECTION ( 'NONE',  ( 0.000000000000000000, 0.000000000000000000, -1.000000000000000000 ) ) ;
#9688 = EDGE_LOOP ( 'NONE', ( #11521, #3783 ) ) ;
#9689 = FACE_OUTER_BOUND ( 'NONE', #11541, .T. ) ;
#9690 = AXIS2_PLACEMENT_3D ( 'NONE', #7495, #8568, #10780 ) ;
#9691 = ORIENTED_EDGE ( 'NONE', *, *, #12502, .F. ) ;
#9692 = CIRCLE ( 'NONE', #3658, 4.250000000000000000 ) ;
#9693 = CONICAL_SURFACE ( 'NONE', #748, 55.00000000000000000, 0.5235987755983000369 ) ;
#9694 = VERTEX_POINT ( 'NONE', #6374 ) ;
#9695 = DIRECTION ( 'NONE',  ( 0.000000000000000000, 0.000000000000000000, -1.000000000000000000 ) ) ;
#9696 = ADVANCED_FACE ( 'NONE', ( #5259 ), #1466, .F. ) ;
#9697 = ORIENTED_EDGE ( 'NONE', *, *, #4600, .F. ) ;
#9698 = CARTESIAN_POINT ( 'NONE',  ( -32.26435573746199736, 42.04772703543562073, -13.00000000000000178 ) ) ;
#9699 = AXIS2_PLACEMENT_3D ( 'NONE', #9784, #8504, #2885 ) ;
#9700 = EDGE_CURVE ( 'NONE', #9830, #11793, #2058, .T. ) ;
#9701 = CARTESIAN_POINT ( 'NONE',  ( 52.54657765281197612, -6.917888187662545540, -8.000000000000000000 ) ) ;
#9702 = FACE_OUTER_BOUND ( 'NONE', #292, .T. ) ;
#9703 = CARTESIAN_POINT ( 'NONE',  ( 2.000000000000008882, -3.464101615137750390, 0.000000000000000000 ) ) ;
#9704 = CIRCLE ( 'NONE', #3182, 107.0000000000000284 ) ;
#9705 = CARTESIAN_POINT ( 'NONE',  ( 13.71740939043365337, -51.19406879332061067, -8.000000000000000000 ) ) ;
#9706 = CIRCLE ( 'NONE', #1964, 2.649999999999985700 ) ;
#9707 = ORIENTED_EDGE ( 'NONE', *, *, #13235, .F. ) ;
#9708 = EDGE_CURVE ( 'NONE', #12909, #10622, #1934, .T. ) ;
#9709 = ORIENTED_EDGE ( 'NONE', *, *, #4455, .F. ) ;
#9710 = CARTESIAN_POINT ( 'NONE',  ( 9.706953719245472456, 57.06275842387054098, -10.50000000000000000 ) ) ;
#9711 = LINE ( 'NONE', #7214, #6606 ) ;
#9712 = AXIS2_PLACEMENT_3D ( 'NONE', #14870, #4617, #6877 ) ;
#9713 = ORIENTED_EDGE ( 'NONE', *, *, #5289, .T. ) ;
#9714 = CARTESIAN_POINT ( 'NONE',  ( -36.14014761921588104, 11.74264578624790190, -25.50000000000000355 ) ) ;
#9715 = AXIS2_PLACEMENT_3D ( 'NONE', #13243, #8592, #1774 ) ;
#9716 = EDGE_CURVE ( 'NONE', #5988, #3770, #9875, .T. ) ;
#9717 = DIRECTION ( 'NONE',  ( -0.000000000000000000, -0.000000000000000000, -1.000000000000000000 ) ) ;
#9718 = EDGE_CURVE ( 'NONE', #8383, #9852, #3884, .T. ) ;
#9719 = VERTEX_POINT ( 'NONE', #7375 ) ;
#9720 = LINE ( 'NONE', #13159, #2171 ) ;
#9721 = ORIENTED_EDGE ( 'NONE', *, *, #4818, .F. ) ;
#9722 = DIRECTION ( 'NONE',  ( -0.000000000000000000, -0.000000000000000000, -1.000000000000000000 ) ) ;
#9723 = CARTESIAN_POINT ( 'NONE',  ( 56.43380494353997534, 12.86891638962136319, -10.50000000000000000 ) ) ;
#9724 = CIRCLE ( 'NONE', #775, 0.5000000000000022204 ) ;
#9725 = DIRECTION ( 'NONE',  ( 1.000000000000000000, -9.769962616701375978E-15, 0.000000000000000000 ) ) ;
#9726 = CARTESIAN_POINT ( 'NONE',  ( -25.00000000000000000, 81.24038404635962252, -31.00000000000000000 ) ) ;
#9727 = EDGE_CURVE ( 'NONE', #8393, #8383, #10907, .T. ) ;
#9728 = CARTESIAN_POINT ( 'NONE',  ( -33.48561063518626923, 47.21331623427104063, -10.50000000000000000 ) ) ;
#9729 = EDGE_LOOP ( 'NONE', ( #9595, #5234, #9975, #2318 ) ) ;
#9730 = VECTOR ( 'NONE', #9466, 1000.000000000000000 ) ;
#9731 = CARTESIAN_POINT ( 'NONE',  ( 12.50000000000000000, 106.2673515243510991, 15.00000000000000000 ) ) ;
#9732 = CARTESIAN_POINT ( 'NONE',  ( -37.12029293941250074, 89.61631465359532456, -13.00000000000000178 ) ) ;
#9733 = UNCERTAINTY_MEASURE_WITH_UNIT (LENGTH_MEASURE( 1.000000000000000082E-05 ), #518, 'distance_accuracy_value', 'NONE');
#9734 = DIRECTION ( 'NONE',  ( 1.000000000000000000, 0.000000000000000000, 0.000000000000000000 ) ) ;
#9735 = AXIS2_PLACEMENT_3D ( 'NONE', #8386, #13250, #10655 ) ;
#9736 = ORIENTED_EDGE ( 'NONE', *, *, #12561, .F. ) ;
#9737 = DIRECTION ( 'NONE',  ( -1.000000000000000000, 0.000000000000000000, 0.000000000000000000 ) ) ;
#9738 = VERTEX_POINT ( 'NONE', #14288 ) ;
#9739 = AXIS2_PLACEMENT_3D ( 'NONE', #13016, #333, #4971 ) ;
#9740 = DIRECTION ( 'NONE',  ( -1.000000000000000000, 0.000000000000000000, 0.000000000000000000 ) ) ;
#9741 = PLANE ( 'NONE',  #6094 ) ;
#9742 = ORIENTED_EDGE ( 'NONE', *, *, #12478, .F. ) ;
#9743 = CARTESIAN_POINT ( 'NONE',  ( -32.46576781417928714, 41.59008834022678514, -10.50000000000000000 ) ) ;
#9744 = DIRECTION ( 'NONE',  ( 1.000000000000000000, 0.000000000000000000, 0.000000000000000000 ) ) ;
#9745 = DIRECTION ( 'NONE',  ( -1.000000000000000000, 0.000000000000000000, 0.000000000000000000 ) ) ;
#9746 = EDGE_LOOP ( 'NONE', ( #13691, #6135 ) ) ;
#9747 = VECTOR ( 'NONE', #8007, 1000.000000000000000 ) ;
#9748 = DIRECTION ( 'NONE',  ( -1.000000000000000000, 0.000000000000000000, 0.000000000000000000 ) ) ;
#9749 = DIRECTION ( 'NONE',  ( 1.000000000000000000, 0.000000000000000000, 0.000000000000000000 ) ) ;
#9750 = DIRECTION ( 'NONE',  ( -0.000000000000000000, -0.000000000000000000, -1.000000000000000000 ) ) ;
#9751 = ORIENTED_EDGE ( 'NONE', *, *, #4545, .T. ) ;
#9752 = AXIS2_PLACEMENT_3D ( 'NONE', #14024, #6792, #8020 ) ;
#9753 = VERTEX_POINT ( 'NONE', #13013 ) ;
#9754 = CARTESIAN_POINT ( 'NONE',  ( -26.49999999999971578, -45.89934640057541060, -8.000000000000000000 ) ) ;
#9755 = ORIENTED_EDGE ( 'NONE', *, *, #8325, .F. ) ;
#9756 = AXIS2_PLACEMENT_3D ( 'NONE', #8511, #14285, #8292 ) ;
#9757 = DIRECTION ( 'NONE',  ( 1.000000000000000000, 0.000000000000000000, 0.000000000000000000 ) ) ;
#9758 = EDGE_CURVE ( 'NONE', #5520, #8464, #7010, .T. ) ;
#9759 = EDGE_CURVE ( 'NONE', #2920, #8250, #482, .T. ) ;
#9760 = CARTESIAN_POINT ( 'NONE',  ( -43.30127018922181037, 25.00000000000021672, -8.000000000000000000 ) ) ;
#9761 = EDGE_CURVE ( 'NONE', #13374, #7769, #9200, .T. ) ;
#9762 = EDGE_CURVE ( 'NONE', #8164, #11760, #3644, .T. ) ;
#9763 = AXIS2_PLACEMENT_3D ( 'NONE', #11661, #10207, #12720 ) ;
#9764 = DIRECTION ( 'NONE',  ( -1.000000000000000000, 0.000000000000000000, 0.000000000000000000 ) ) ;
#9765 = DIRECTION ( 'NONE',  ( 0.000000000000000000, 0.000000000000000000, 1.000000000000000000 ) ) ;
#9766 = ORIENTED_EDGE ( 'NONE', *, *, #8850, .T. ) ;
#9767 = DIRECTION ( 'NONE',  ( 1.000000000000000000, 0.000000000000000000, 0.000000000000000000 ) ) ;
#9768 = AXIS2_PLACEMENT_3D ( 'NONE', #6118, #3708, #8407 ) ;
#9769 = ORIENTED_EDGE ( 'NONE', *, *, #6464, .F. ) ;
#9770 = VERTEX_POINT ( 'NONE', #1687 ) ;
#9771 = CARTESIAN_POINT ( 'NONE',  ( 33.48561063518626923, -47.21331623427104063, -8.000000000000000000 ) ) ;
#9772 = VECTOR ( 'NONE', #9717, 1000.000000000000000 ) ;
#9773 = EDGE_LOOP ( 'NONE', ( #1151, #5283, #12730, #9282 ) ) ;
#9774 = AXIS2_PLACEMENT_3D ( 'NONE', #13307, #12258, #1848 ) ;
#9775 = CARTESIAN_POINT ( 'NONE',  ( -31.05588327715806329, 44.79355920668842828, 8.000000000000000000 ) ) ;
#9776 = CYLINDRICAL_SURFACE ( 'NONE', #10036, 5.000000000000000000 ) ;
#9777 = CARTESIAN_POINT ( 'NONE',  ( 0.000000000000000000, 0.000000000000000000, -10.50000000000000000 ) ) ;
#9778 = CARTESIAN_POINT ( 'NONE',  ( 6.917888187663118416, 52.54657765281190507, -13.00000000000000178 ) ) ;
#9779 = EDGE_CURVE ( 'NONE', #13295, #8252, #9720, .T. ) ;
#9780 = DIRECTION ( 'NONE',  ( 1.000000000000000000, 0.000000000000000000, 0.000000000000000000 ) ) ;
#9781 = ORIENTED_EDGE ( 'NONE', *, *, #10386, .F. ) ;
#9782 = VECTOR ( 'NONE', #14207, 1000.000000000000114 ) ;
#9783 = AXIS2_PLACEMENT_3D ( 'NONE', #6490, #9844, #14488 ) ;
#9784 = CARTESIAN_POINT ( 'NONE',  ( 30.80502811811196295, 49.00442420936003174, -10.50000000000000000 ) ) ;
#9785 = CIRCLE ( 'NONE', #3262, 59.50000000000000000 ) ;
#9786 = LINE ( 'NONE', #12445, #4562 ) ;
#9787 = EDGE_CURVE ( 'NONE', #12536, #7623, #8662, .T. ) ;
#9788 = CARTESIAN_POINT ( 'NONE',  ( 37.12029293941315444, -89.61631465359504034, 10.49999999999999822 ) ) ;
#9789 = DIRECTION ( 'NONE',  ( 0.000000000000000000, 0.000000000000000000, -1.000000000000000000 ) ) ;
#9790 = ORIENTED_EDGE ( 'NONE', *, *, #11323, .T. ) ;
#9791 = DIRECTION ( 'NONE',  ( 1.000000000000000000, 0.000000000000000000, 0.000000000000000000 ) ) ;
#9792 = EDGE_LOOP ( 'NONE', ( #13757, #1166, #7704, #827 ) ) ;
#9793 = CIRCLE ( 'NONE', #11284, 3.000000000000002665 ) ;
#9794 = DIRECTION ( 'NONE',  ( 0.000000000000000000, 0.000000000000000000, 1.000000000000000000 ) ) ;
#9795 = ORIENTED_EDGE ( 'NONE', *, *, #10515, .F. ) ;
#9796 = VECTOR ( 'NONE', #13030, 1000.000000000000000 ) ;
#9797 = VECTOR ( 'NONE', #1480, 1000.000000000000000 ) ;
#9798 = CARTESIAN_POINT ( 'NONE',  ( 0.000000000000000000, 0.000000000000000000, 8.000000000000000000 ) ) ;
#9799 = CIRCLE ( 'NONE', #9081, 0.5000000000000043299 ) ;
#9800 = ORIENTED_EDGE ( 'NONE', *, *, #8709, .T. ) ;
#9801 = CARTESIAN_POINT ( 'NONE',  ( 12.23689275498546536, 106.2979809871390415, 16.60898801976832573 ) ) ;
#9802 = CYLINDRICAL_SURFACE ( 'NONE', #2421, 3.000000000000002665 ) ;
#9803 = CARTESIAN_POINT ( 'NONE',  ( 5.000000000000007105, 85.00000000000000000, 46.00000000000000000 ) ) ;
#9804 = CARTESIAN_POINT ( 'NONE',  ( 2.500000000000002220, 0.000000000000000000, 0.000000000000000000 ) ) ;
#9805 = DIRECTION ( 'NONE',  ( -1.000000000000000000, 0.000000000000000000, 0.000000000000000000 ) ) ;
#9806 = DIRECTION ( 'NONE',  ( -0.000000000000000000, -0.000000000000000000, -1.000000000000000000 ) ) ;
#9807 = EDGE_CURVE ( 'NONE', #7876, #669, #14547, .T. ) ;
#9808 = VECTOR ( 'NONE', #14443, 1000.000000000000000 ) ;
#9809 = ORIENTED_EDGE ( 'NONE', *, *, #14721, .T. ) ;
#9810 = EDGE_CURVE ( 'NONE', #8471, #4116, #5328, .T. ) ;
#9811 = CIRCLE ( 'NONE', #12501, 63.00000000000000000 ) ;
#9812 = CARTESIAN_POINT ( 'NONE',  ( 47.21331623427115431, 33.48561063518610581, -10.50000000000000000 ) ) ;
#9813 = CYLINDRICAL_SURFACE ( 'NONE', #850, 56.99999999999999289 ) ;
#9814 = VECTOR ( 'NONE', #14886, 1000.000000000000000 ) ;
#9815 = EDGE_CURVE ( 'NONE', #721, #13514, #10897, .T. ) ;
#9816 = CARTESIAN_POINT ( 'NONE',  ( -29.70588235294118107, 96.53269163155674448, -79.80561291909842225 ) ) ;
#9817 = ORIENTED_EDGE ( 'NONE', *, *, #3411, .T. ) ;
#9818 = PRODUCT_DEFINITION_CONTEXT ( 'detailed design', #13871, 'design' ) ;
#9819 = ORIENTED_EDGE ( 'NONE', *, *, #5816, .F. ) ;
#9820 = EDGE_CURVE ( 'NONE', #1055, #12316, #14447, .T. ) ;
#9821 = CARTESIAN_POINT ( 'NONE',  ( -4.175002511812149208, -2.208363329454906765, -3.469254087858247626 ) ) ;
#9822 = CIRCLE ( 'NONE', #3789, 0.5000000000000004441 ) ;
#9823 = ORIENTED_EDGE ( 'NONE', *, *, #2165, .T. ) ;
#9824 = CARTESIAN_POINT ( 'NONE',  ( -52.50000000000000711, 0.000000000000000000, -13.00000000000000178 ) ) ;
#9825 = CARTESIAN_POINT ( 'NONE',  ( -12.07490296461408974, 74.02221379130672574, 17.09816637537096540 ) ) ;
#9826 = CARTESIAN_POINT ( 'NONE',  ( 7.500000000000000000, 106.7368258849775202, 20.00000000000000355 ) ) ;
#9827 = CARTESIAN_POINT ( 'NONE',  ( 12.50000000000000000, 40.62019202317980415, -31.00000000000000000 ) ) ;
#9828 = CARTESIAN_POINT ( 'NONE',  ( -12.50000000000000000, 40.62019202317981126, 23.50000000000000355 ) ) ;
#9829 = EDGE_LOOP ( 'NONE', ( #10140, #1651, #5602, #3964, #5689, #2792, #4014, #8805, #5224, #650, #13985 ) ) ;
#9830 = VERTEX_POINT ( 'NONE', #11954 ) ;
#9831 = ADVANCED_FACE ( 'NONE', ( #7446 ), #12095, .F. ) ;
#9832 = AXIS2_PLACEMENT_3D ( 'NONE', #2016, #12426, #4235 ) ;
#9833 = DIRECTION ( 'NONE',  ( -1.000000000000000000, 1.065814103640150279E-14, 0.000000000000000000 ) ) ;
#9834 = DIRECTION ( 'NONE',  ( -0.000000000000000000, -0.000000000000000000, 1.000000000000000000 ) ) ;
#9835 = AXIS2_PLACEMENT_3D ( 'NONE', #2404, #12750, #3858 ) ;
#9836 = DIRECTION ( 'NONE',  ( 0.000000000000000000, 0.000000000000000000, 1.000000000000000000 ) ) ;
#9837 = ORIENTED_EDGE ( 'NONE', *, *, #2631, .T. ) ;
#9838 = EDGE_LOOP ( 'NONE', ( #2786, #14540, #3591, #10725 ) ) ;
#9839 = FACE_OUTER_BOUND ( 'NONE', #6259, .T. ) ;
#9840 = ORIENTED_EDGE ( 'NONE', *, *, #11705, .T. ) ;
#9841 = CIRCLE ( 'NONE', #4521, 3.000000000000002665 ) ;
#9842 = DIRECTION ( 'NONE',  ( -1.000000000000000000, 0.000000000000000000, 0.000000000000000000 ) ) ;
#9843 = PRODUCT_DEFINITION_SHAPE ( 'NONE', 'NONE',  #15032 ) ;
#9844 = DIRECTION ( 'NONE',  ( 0.000000000000000000, 0.000000000000000000, -1.000000000000000000 ) ) ;
#9845 = ORIENTED_EDGE ( 'NONE', *, *, #5903, .T. ) ;
#9846 = DIRECTION ( 'NONE',  ( 1.000000000000000000, 0.000000000000000000, 0.000000000000000000 ) ) ;
#9847 = CARTESIAN_POINT ( 'NONE',  ( -31.72333741318944433, 102.1879147510518919, 12.61437971294004790 ) ) ;
#9848 = ORIENTED_EDGE ( 'NONE', *, *, #3345, .F. ) ;
#9849 = VECTOR ( 'NONE', #5379, 1000.000000000000000 ) ;
#9850 = CARTESIAN_POINT ( 'NONE',  ( 2.000000000000008882, -3.464101615137750390, 0.000000000000000000 ) ) ;
#9851 = AXIS2_PLACEMENT_3D ( 'NONE', #625, #12239, #2887 ) ;
#9852 = VERTEX_POINT ( 'NONE', #8813 ) ;
#9853 = ORIENTED_EDGE ( 'NONE', *, *, #4743, .T. ) ;
#9854 = CARTESIAN_POINT ( 'NONE',  ( 18.52941176470587692, 60.21346111671358159, 26.00000000000000000 ) ) ;
#9855 = EDGE_CURVE ( 'NONE', #14546, #10333, #4842, .T. ) ;
#9856 = EDGE_CURVE ( 'NONE', #7413, #4919, #13326, .T. ) ;
#9857 = DIRECTION ( 'NONE',  ( -0.000000000000000000, -0.000000000000000000, 1.000000000000000000 ) ) ;
#9858 = CARTESIAN_POINT ( 'NONE',  ( -6.917888187662729393, -52.54657765281195481, 8.000000000000000000 ) ) ;
#9859 = CARTESIAN_POINT ( 'NONE',  ( -31.74999999999995737, 0.000000000000000000, -2.775557561562891351E-14 ) ) ;
#9860 = DIRECTION ( 'NONE',  ( 0.000000000000000000, 0.000000000000000000, -1.000000000000000000 ) ) ;
#9861 = CARTESIAN_POINT ( 'NONE',  ( 92.55687898036906347, 36.52608637591612961, -13.00000000000000178 ) ) ;
#9862 = ORIENTED_EDGE ( 'NONE', *, *, #14511, .T. ) ;
#9863 = ORIENTED_EDGE ( 'NONE', *, *, #9870, .F. ) ;
#9864 = LINE ( 'NONE', #6880, #9873 ) ;
#9865 = EDGE_CURVE ( 'NONE', #2732, #132, #2662, .T. ) ;
#9866 = DIRECTION ( 'NONE',  ( 1.000000000000000000, 0.000000000000000000, 0.000000000000000000 ) ) ;
#9867 = CARTESIAN_POINT ( 'NONE',  ( -0.6920835326022556355, -4.454600218803903999, -3.597382984111584747 ) ) ;
#9868 = ORIENTED_EDGE ( 'NONE', *, *, #8934, .T. ) ;
#9869 = DIRECTION ( 'NONE',  ( 0.000000000000000000, 0.000000000000000000, 1.000000000000000000 ) ) ;
#9870 = EDGE_CURVE ( 'NONE', #14678, #7442, #3654, .T. ) ;
#9871 = ORIENTED_EDGE ( 'NONE', *, *, #8649, .T. ) ;
#9872 = LINE ( 'NONE', #11101, #11261 ) ;
#9873 = VECTOR ( 'NONE', #913, 1000.000000000000000 ) ;
#9874 = ORIENTED_EDGE ( 'NONE', *, *, #8625, .F. ) ;
#9875 = LINE ( 'NONE', #633, #6038 ) ;
#9876 = ORIENTED_EDGE ( 'NONE', *, *, #10554, .T. ) ;
#9877 = DIRECTION ( 'NONE',  ( 0.000000000000000000, 0.000000000000000000, 1.000000000000000000 ) ) ;
#9878 = CARTESIAN_POINT ( 'NONE',  ( 11.55014193876178297, -53.26842454702432406, -8.000000000000000000 ) ) ;
#9879 = CYLINDRICAL_SURFACE ( 'NONE', #5868, 4.250000000000000000 ) ;
#9880 = CARTESIAN_POINT ( 'NONE',  ( -9.706953719245875689, -57.06275842387046993, 10.49999999999999822 ) ) ;
#9881 = DIRECTION ( 'NONE',  ( 1.000000000000000000, 0.000000000000000000, 0.000000000000000000 ) ) ;
#9882 = DIRECTION ( 'NONE',  ( 0.000000000000000000, 0.000000000000000000, -1.000000000000000000 ) ) ;
#9883 = AXIS2_PLACEMENT_3D ( 'NONE', #9528, #14178, #3627 ) ;
#9884 = ORIENTED_EDGE ( 'NONE', *, *, #1518, .T. ) ;
#9885 = DIRECTION ( 'NONE',  ( 1.000000000000000000, 0.000000000000000000, 0.000000000000000000 ) ) ;
#9886 = PLANE ( 'NONE',  #7851 ) ;
#9887 = CYLINDRICAL_SURFACE ( 'NONE', #813, 0.5000000000000004441 ) ;
#9888 = VERTEX_POINT ( 'NONE', #13681 ) ;
#9889 = CARTESIAN_POINT ( 'NONE',  ( 0.000000000000000000, 0.000000000000000000, 8.000000000000000000 ) ) ;
#9890 = EDGE_CURVE ( 'NONE', #10669, #2752, #11163, .T. ) ;
#9891 = ADVANCED_FACE ( 'NONE', ( #13524 ), #862, .T. ) ;
#9892 = VERTEX_POINT ( 'NONE', #8734 ) ;
#9893 = EDGE_CURVE ( 'NONE', #1264, #14119, #2427, .T. ) ;
#9894 = DIRECTION ( 'NONE',  ( 1.000000000000000000, 0.000000000000000000, 0.000000000000000000 ) ) ;
#9895 = FILL_AREA_STYLE ('',( #13477 ) ) ;
#9896 = ORIENTED_EDGE ( 'NONE', *, *, #11310, .T. ) ;
#9897 = CARTESIAN_POINT ( 'NONE',  ( -33.48561063518626923, 47.21331623427104063, -10.50000000000000000 ) ) ;
#9898 = LINE ( 'NONE', #12419, #6614 ) ;
#9899 = DIRECTION ( 'NONE',  ( 0.000000000000000000, 0.000000000000000000, 1.000000000000000000 ) ) ;
#9900 = VERTEX_POINT ( 'NONE', #3129 ) ;
#9901 = VERTEX_POINT ( 'NONE', #5325 ) ;
#9902 = ORIENTED_EDGE ( 'NONE', *, *, #11333, .F. ) ;
#9903 = ADVANCED_FACE ( 'NONE', ( #12547 ), #14603, .F. ) ;
#9904 = DIRECTION ( 'NONE',  ( -0.9557692240748190127, -0.2941176470588235392, -5.100557892117772022E-16 ) ) ;
#9905 = DIRECTION ( 'NONE',  ( 0.000000000000000000, 0.000000000000000000, -1.000000000000000000 ) ) ;
#9906 = CARTESIAN_POINT ( 'NONE',  ( 53.26842454702428142, 11.55014193876197126, -13.00000000000000178 ) ) ;
#9907 = ORIENTED_EDGE ( 'NONE', *, *, #8142, .F. ) ;
#9908 = CONICAL_SURFACE ( 'NONE', #3371, 2.041999999999999815, 1.047197551196591858 ) ;
#9909 = ORIENTED_EDGE ( 'NONE', *, *, #3385, .T. ) ;
#9910 = VERTEX_POINT ( 'NONE', #7903 ) ;
#9911 = EDGE_CURVE ( 'NONE', #2565, #14269, #6522, .T. ) ;
#9912 = ORIENTED_EDGE ( 'NONE', *, *, #8110, .F. ) ;
#9913 = ADVANCED_FACE ( 'NONE', ( #6747 ), #13456, .F. ) ;
#9914 = CARTESIAN_POINT ( 'NONE',  ( -30.80502811811232888, -49.00442420935981147, -13.00000000000000178 ) ) ;
#9915 = AXIS2_PLACEMENT_3D ( 'NONE', #4150, #11208, #6249 ) ;
#9916 = CARTESIAN_POINT ( 'NONE',  ( 0.000000000000000000, 0.000000000000000000, -8.000000000000000000 ) ) ;
#9917 =( NAMED_UNIT ( * ) SI_UNIT ( $, .STERADIAN. ) SOLID_ANGLE_UNIT ( ) );
#9918 = CARTESIAN_POINT ( 'NONE',  ( -1.674280531759324342, -99.48933418828643482, -8.000000000000000000 ) ) ;
#9919 = CIRCLE ( 'NONE', #7978, 52.50000000000000711 ) ;
#9920 = ORIENTED_EDGE ( 'NONE', *, *, #3480, .T. ) ;
#9921 = DIRECTION ( 'NONE',  ( 0.000000000000000000, 0.000000000000000000, 1.000000000000000000 ) ) ;
#9922 = CARTESIAN_POINT ( 'NONE',  ( 86.67575032682076142, 37.71449950291080455, -8.000000000000000000 ) ) ;
#9923 = VERTEX_POINT ( 'NONE', #7599 ) ;
#9924 = CARTESIAN_POINT ( 'NONE',  ( 5.000000000000007105, 85.00000000000000000, 31.00000000000000000 ) ) ;
#9925 = ORIENTED_EDGE ( 'NONE', *, *, #9597, .T. ) ;
#9926 = AXIS2_PLACEMENT_3D ( 'NONE', #2706, #9599, #1269 ) ;
#9927 = AXIS2_PLACEMENT_3D ( 'NONE', #13428, #6578, #11233 ) ;
#9928 = ORIENTED_EDGE ( 'NONE', *, *, #11408, .T. ) ;
#9929 = CARTESIAN_POINT ( 'NONE',  ( -32.78625152019765920, 95.53054288192238630, 15.68243957109766207 ) ) ;
#9930 = CIRCLE ( 'NONE', #3396, 7.500000000000001776 ) ;
#9931 = CIRCLE ( 'NONE', #9682, 60.50000000000000000 ) ;
#9932 = CARTESIAN_POINT ( 'NONE',  ( 0.000000000000000000, 0.000000000000000000, 8.000000000000000000 ) ) ;
#9933 = CARTESIAN_POINT ( 'NONE',  ( 0.000000000000000000, 0.000000000000000000, -8.000000000000000000 ) ) ;
#9934 = DIRECTION ( 'NONE',  ( 0.000000000000000000, 0.000000000000000000, 1.000000000000000000 ) ) ;
#9935 = CARTESIAN_POINT ( 'NONE',  ( -2.712762565639317280, 3.052587955997805302, -3.430618716626997688 ) ) ;
#9936 = AXIS2_PLACEMENT_3D ( 'NONE', #12470, #6600, #12251 ) ;
#9937 = CARTESIAN_POINT ( 'NONE',  ( -33.47282819776587814, 39.30189486418276346, 8.000000000000000000 ) ) ;
#9938 = ORIENTED_EDGE ( 'NONE', *, *, #10427, .T. ) ;
#9939 = AXIS2_PLACEMENT_3D ( 'NONE', #10038, #4432, #1993 ) ;
#9940 = ADVANCED_FACE ( 'NONE', ( #7824 ), #4349, .T. ) ;
#9941 = AXIS2_PLACEMENT_3D ( 'NONE', #7299, #10805, #6086 ) ;
#9942 = FACE_BOUND ( 'NONE', #10070, .T. ) ;
#9943 = VERTEX_POINT ( 'NONE', #14752 ) ;
#9944 = MECHANICAL_DESIGN_GEOMETRIC_PRESENTATION_REPRESENTATION (  '', ( #13589 ), #502 ) ;
#9945 = DIRECTION ( 'NONE',  ( 0.000000000000000000, 0.000000000000000000, -1.000000000000000000 ) ) ;
#9946 = CARTESIAN_POINT ( 'NONE',  ( -97.00000000000000000, 1.015776140243522349E-12, -13.00000000000000178 ) ) ;
#9947 = ORIENTED_EDGE ( 'NONE', *, *, #5878, .T. ) ;
#9948 = CARTESIAN_POINT ( 'NONE',  ( 32.35652065542060285, 95.67730775537752663, -15.49454652436121727 ) ) ;
#9949 = ORIENTED_EDGE ( 'NONE', *, *, #13441, .F. ) ;
#9950 = AXIS2_PLACEMENT_3D ( 'NONE', #1286, #3410, #5900 ) ;
#9951 = CARTESIAN_POINT ( 'NONE',  ( 0.000000000000000000, 0.000000000000000000, -28.00000000000000000 ) ) ;
#9952 = ORIENTED_EDGE ( 'NONE', *, *, #10847, .T. ) ;
#9953 = CARTESIAN_POINT ( 'NONE',  ( -51.19406879332065330, -13.71740939043347041, 8.000000000000000000 ) ) ;
#9954 = VECTOR ( 'NONE', #455, 1000.000000000000000 ) ;
#9955 = VERTEX_POINT ( 'NONE', #1905 ) ;
#9956 = AXIS2_PLACEMENT_3D ( 'NONE', #10997, #3945, #6266 ) ;
#9957 = CARTESIAN_POINT ( 'NONE',  ( -51.19406879332065330, -13.71740939043347041, -13.00000000000000178 ) ) ;
#9958 = DIRECTION ( 'NONE',  ( 0.000000000000000000, 0.000000000000000000, 1.000000000000000000 ) ) ;
#9959 = LINE ( 'NONE', #4287, #10721 ) ;
#9960 = CARTESIAN_POINT ( 'NONE',  ( -52.54657765281192638, 6.917888187662934563, -13.00000000000000178 ) ) ;
#9961 = EDGE_CURVE ( 'NONE', #5756, #7182, #11179, .T. ) ;
#9962 = PLANE ( 'NONE',  #9774 ) ;
#9963 = EDGE_CURVE ( 'NONE', #12145, #13693, #1009, .T. ) ;
#9964 = EDGE_CURVE ( 'NONE', #13797, #7984, #4025, .T. ) ;
#9965 = DIRECTION ( 'NONE',  ( 0.000000000000000000, 0.000000000000000000, 1.000000000000000000 ) ) ;
#9966 = CIRCLE ( 'NONE', #13861, 3.000000000000002665 ) ;
#9967 = ORIENTED_EDGE ( 'NONE', *, *, #10753, .F. ) ;
#9968 = CARTESIAN_POINT ( 'NONE',  ( 12.50000000000000000, 40.62019202317980415, 31.00000000000000000 ) ) ;
#9969 = AXIS2_PLACEMENT_3D ( 'NONE', #10223, #6870, #10302 ) ;
#9970 = CARTESIAN_POINT ( 'NONE',  ( -39.66766701456180755, -30.43807145043597728, 8.000000000000000000 ) ) ;
#9971 = CIRCLE ( 'NONE', #2941, 63.00000000000000000 ) ;
#9972 = CARTESIAN_POINT ( 'NONE',  ( -2.449293598294708880E-16, 38.00000000000000000, -25.50000000000000355 ) ) ;
#9973 = EDGE_CURVE ( 'NONE', #3062, #3301, #11422, .T. ) ;
#9974 = PRODUCT_DEFINITION_SHAPE ( 'NONE', 'NONE',  #15043 ) ;
#9975 = ORIENTED_EDGE ( 'NONE', *, *, #13676, .F. ) ;
#9976 = APPLICATION_CONTEXT ( 'automotive_design' ) ;
#9977 = DIRECTION ( 'NONE',  ( -1.000000000000000000, 4.163336342344304841E-14, 0.000000000000000000 ) ) ;
#9978 = ORIENTED_EDGE ( 'NONE', *, *, #8531, .F. ) ;
#9979 = DIRECTION ( 'NONE',  ( 1.000000000000000000, 0.000000000000000000, 0.000000000000000000 ) ) ;
#9980 = DIRECTION ( 'NONE',  ( -0.000000000000000000, -0.000000000000000000, 1.000000000000000000 ) ) ;
#9981 = CIRCLE ( 'NONE', #11970, 0.5000000000000004441 ) ;
#9982 = CARTESIAN_POINT ( 'NONE',  ( -9.714003807513870825, -53.63365512954690217, 8.000000000000000000 ) ) ;
#9983 = CIRCLE ( 'NONE', #14851, 3.000000000000002665 ) ;
#9984 = DIRECTION ( 'NONE',  ( -1.000000000000000000, 0.000000000000000000, 0.000000000000000000 ) ) ;
#9985 = APPLICATION_PROTOCOL_DEFINITION ( 'draft international standard', 'automotive_design', 1998, #1442 ) ;
#9986 = EDGE_LOOP ( 'NONE', ( #7164, #13377, #12001, #2874, #11199 ) ) ;
#9987 = EDGE_LOOP ( 'NONE', ( #13052, #6540, #7233, #9650, #11228, #3995 ) ) ;
#9988 = CARTESIAN_POINT ( 'NONE',  ( 5.196599455413437438E-15, 4.647089433458989838, -3.572167766733754135 ) ) ;
#9989 = CARTESIAN_POINT ( 'NONE',  ( -29.49928053175900899, -45.83364790889059037, -8.000000000000000000 ) ) ;
#9990 = AXIS2_PLACEMENT_3D ( 'NONE', #11095, #4420, #7893 ) ;
#9991 = EDGE_CURVE ( 'NONE', #1689, #8733, #4870, .T. ) ;
#9992 = DIRECTION ( 'NONE',  ( -1.000000000000000000, 0.000000000000000000, 0.000000000000000000 ) ) ;
#9993 = ORIENTED_EDGE ( 'NONE', *, *, #6845, .F. ) ;
#9994 = VERTEX_POINT ( 'NONE', #9118 ) ;
#9995 = ORIENTED_EDGE ( 'NONE', *, *, #4589, .T. ) ;
#9996 = ORIENTED_EDGE ( 'NONE', *, *, #13575, .T. ) ;
#9997 = CARTESIAN_POINT ( 'NONE',  ( -12.50000000000000000, 100.2235002382176248, -15.33678752976415716 ) ) ;
#9998 = AXIS2_PLACEMENT_3D ( 'NONE', #1555, #3688, #11968 ) ;
#9999 = CARTESIAN_POINT ( 'NONE',  ( 50.13108361037843252, 56.43380494353993271, 8.000000000000000000 ) ) ;
#10000 = CARTESIAN_POINT ( 'NONE',  ( -2.500000000000000444, 3.061616997868383634E-16, -25.03750572909317285 ) ) ;
#10001 = ORIENTED_EDGE ( 'NONE', *, *, #6890, .F. ) ;
#10002 = CARTESIAN_POINT ( 'NONE',  ( 25.00000000000000000, 81.24038404635960831, 26.00000000000000000 ) ) ;
#10003 = CARTESIAN_POINT ( 'NONE',  ( -33.82975856321728969, 101.3925934381291256, 15.34957766734057927 ) ) ;
#10004 = VERTEX_POINT ( 'NONE', #2426 ) ;
#10005 = FACE_OUTER_BOUND ( 'NONE', #4230, .T. ) ;
#10006 = ADVANCED_FACE ( 'NONE', ( #7050 ), #12144, .T. ) ;
#10007 = EDGE_CURVE ( 'NONE', #7249, #8663, #994, .T. ) ;
#10008 = ORIENTED_EDGE ( 'NONE', *, *, #9392, .F. ) ;
#10009 = VECTOR ( 'NONE', #7531, 1000.000000000000000 ) ;
#10010 = ORIENTED_EDGE ( 'NONE', *, *, #4678, .T. ) ;
#10011 = CARTESIAN_POINT ( 'NONE',  ( -30.88479107129467849, 96.16227383530475947, 14.30703002621670095 ) ) ;
#10012 = DIRECTION ( 'NONE',  ( 0.000000000000000000, 0.000000000000000000, 1.000000000000000000 ) ) ;
#10013 = EDGE_CURVE ( 'NONE', #10294, #11817, #3653, .T. ) ;
#10014 = AXIS2_PLACEMENT_3D ( 'NONE', #3392, #5592, #10224 ) ;
#10015 = UNCERTAINTY_MEASURE_WITH_UNIT (LENGTH_MEASURE( 1.000000000000000082E-05 ), #7698, 'distance_accuracy_value', 'NONE');
#10016 = CARTESIAN_POINT ( 'NONE',  ( 49.00442420935993226, -30.80502811811213704, 10.49999999999999822 ) ) ;
#10017 = CARTESIAN_POINT ( 'NONE',  ( -12.86891638962156215, 56.43380494353993271, -10.50000000000000000 ) ) ;
#10018 = CARTESIAN_POINT ( 'NONE',  ( 0.000000000000000000, 0.000000000000000000, 8.000000000000000000 ) ) ;
#10019 = CONICAL_SURFACE ( 'NONE', #5424, 52.83493649053890806, 0.5235987755983000369 ) ;
#10020 = ORIENTED_EDGE ( 'NONE', *, *, #1167, .F. ) ;
#10021 = CARTESIAN_POINT ( 'NONE',  ( 0.000000000000000000, 0.000000000000000000, -13.00000000000000178 ) ) ;
#10022 = EDGE_CURVE ( 'NONE', #8852, #14881, #13614, .T. ) ;
#10023 = DIRECTION ( 'NONE',  ( 0.000000000000000000, 0.000000000000000000, -1.000000000000000000 ) ) ;
#10024 = CARTESIAN_POINT ( 'NONE',  ( 2.500000000000002220, -1.178949249685208533, 2.042000000000002036 ) ) ;
#10025 = ORIENTED_EDGE ( 'NONE', *, *, #1834, .F. ) ;
#10026 = LINE ( 'NONE', #8884, #9808 ) ;
#10027 = LINE ( 'NONE', #10946, #14656 ) ;
#10028 = ORIENTED_EDGE ( 'NONE', *, *, #10135, .T. ) ;
#10029 = CARTESIAN_POINT ( 'NONE',  ( 51.53979475227119167, 13.35619814848851483, -13.00000000000000178 ) ) ;
#10030 = ORIENTED_EDGE ( 'NONE', *, *, #4911, .F. ) ;
#10031 = ORIENTED_EDGE ( 'NONE', *, *, #6900, .F. ) ;
#10032 = DIRECTION ( 'NONE',  ( 1.000000000000000000, 0.000000000000000000, 0.000000000000000000 ) ) ;
#10033 = CARTESIAN_POINT ( 'NONE',  ( 45.89934640057532533, -26.49999999999987566, 8.000000000000000000 ) ) ;
#10034 = DIRECTION ( 'NONE',  ( 1.000000000000000000, 0.000000000000000000, 0.000000000000000000 ) ) ;
#10035 = CIRCLE ( 'NONE', #2515, 3.000000000000002665 ) ;
#10036 = AXIS2_PLACEMENT_3D ( 'NONE', #10160, #4414, #845 ) ;
#10037 = VECTOR ( 'NONE', #1329, 1000.000000000000000 ) ;
#10038 = CARTESIAN_POINT ( 'NONE',  ( -33.48561063518626923, 47.21331623427104063, 10.49999999999999822 ) ) ;
#10039 = CARTESIAN_POINT ( 'NONE',  ( 47.21331623427115431, 33.48561063518610581, -10.50000000000000000 ) ) ;
#10040 = CARTESIAN_POINT ( 'NONE',  ( -89.61631465359519666, -37.12029293941281338, 10.49999999999999822 ) ) ;
#10041 = ORIENTED_EDGE ( 'NONE', *, *, #12434, .F. ) ;
#10042 = DIRECTION ( 'NONE',  ( -1.000000000000000000, 0.000000000000000000, 0.000000000000000000 ) ) ;
#10043 = CARTESIAN_POINT ( 'NONE',  ( -50.84834283437000835, -14.07862063237876704, 10.49999999999999822 ) ) ;
#10044 = DIRECTION ( 'NONE',  ( 1.000000000000000000, 0.000000000000000000, 0.000000000000000000 ) ) ;
#10045 = CIRCLE ( 'NONE', #110, 59.50000000000000000 ) ;
#10046 = AXIS2_PLACEMENT_3D ( 'NONE', #646, #7458, #6097 ) ;
#10047 = AXIS2_PLACEMENT_3D ( 'NONE', #635, #12876, #7603 ) ;
#10048 = EDGE_LOOP ( 'NONE', ( #9556, #7428, #14709, #2745, #12409 ) ) ;
#10049 = EDGE_CURVE ( 'NONE', #7502, #12871, #13583, .T. ) ;
#10050 = DIRECTION ( 'NONE',  ( 0.000000000000000000, 0.000000000000000000, 1.000000000000000000 ) ) ;
#10051 = EDGE_CURVE ( 'NONE', #9770, #8885, #12615, .T. ) ;
#10052 = ORIENTED_EDGE ( 'NONE', *, *, #4809, .T. ) ;
#10053 = FACE_OUTER_BOUND ( 'NONE', #3677, .T. ) ;
#10054 = DIRECTION ( 'NONE',  ( -0.2941176470588238168, 0.9557692240748187906, -0.000000000000000000 ) ) ;
#10055 = AXIS2_PLACEMENT_3D ( 'NONE', #9754, #13616, #2717 ) ;
#10056 = DIRECTION ( 'NONE',  ( 0.000000000000000000, 0.000000000000000000, 1.000000000000000000 ) ) ;
#10057 = LINE ( 'NONE', #3086, #1300 ) ;
#10058 = AXIS2_PLACEMENT_3D ( 'NONE', #7854, #13794, #13554 ) ;
#10059 = ITEM_DEFINED_TRANSFORMATION ( 'NONE', 'NONE', #9926,  #5108 ) ;
#10060 = ORIENTED_EDGE ( 'NONE', *, *, #4262, .T. ) ;
#10061 = VECTOR ( 'NONE', #12495, 1000.000000000000000 ) ;
#10062 = AXIS2_PLACEMENT_3D ( 'NONE', #14618, #3297, #4215 ) ;
#10063 = EDGE_CURVE ( 'NONE', #13418, #14780, #6, .T. ) ;
#10064 = ORIENTED_EDGE ( 'NONE', *, *, #7306, .T. ) ;
#10065 = ORIENTED_EDGE ( 'NONE', *, *, #11192, .F. ) ;
#10066 = CARTESIAN_POINT ( 'NONE',  ( 0.000000000000000000, 0.000000000000000000, -13.00000000000000178 ) ) ;
#10067 = DIRECTION ( 'NONE',  ( 0.000000000000000000, 0.000000000000000000, 1.000000000000000000 ) ) ;
#10068 = EDGE_CURVE ( 'NONE', #8464, #10287, #7511, .T. ) ;
#10069 = DIRECTION ( 'NONE',  ( -1.000000000000000000, 3.530314442338765862E-15, 0.000000000000000000 ) ) ;
#10070 = EDGE_LOOP ( 'NONE', ( #4307, #1779 ) ) ;
#10071 = AXIS2_PLACEMENT_3D ( 'NONE', #1444, #2424, #12912 ) ;
#10072 = VERTEX_POINT ( 'NONE', #3585 ) ;
#10073 = EDGE_CURVE ( 'NONE', #1517, #13137, #10919, .T. ) ;
#10074 = AXIS2_PLACEMENT_3D ( 'NONE', #10468, #12901, #10611 ) ;
#10075 = ORIENTED_EDGE ( 'NONE', *, *, #10285, .T. ) ;
#10076 = B_SPLINE_CURVE_WITH_KNOTS ( 'NONE', 3,
 ( #1670, #14347, #3954, #8355, #7431, #1447, #10707, #12079, #6276, #12997, #10925, #531, #14272, #2585, #4032, #2657, #310, #8643, #7275, #13284 ),
 .UNSPECIFIED., .F., .F.,
 ( 4, 2, 2, 2, 2, 2, 2, 2, 2, 4 ),
 ( 0.000000000000000000, 0.0009815662899613894401, 0.001472349434942086871, 0.001963132579922784084, 0.002944698869884174175, 0.003926265159845563832, 0.004907831449806954356, 0.005889397739768344013, 0.006870964029729732803, 0.007852530319691122460 ),
 .UNSPECIFIED. ) ;
#10077 = CARTESIAN_POINT ( 'NONE',  ( -12.39897948556635754, 100.2360479454198696, 16.00000000000000000 ) ) ;
#10078 = CARTESIAN_POINT ( 'NONE',  ( 0.5000000000000045519, -97.00000000000000000, 10.49999999999999822 ) ) ;
#10079 = SURFACE_STYLE_FILL_AREA ( #14725 ) ;
#10080 = CARTESIAN_POINT ( 'NONE',  ( -12.50000000000000000, 100.2235002382176248, 15.00000000000000000 ) ) ;
#10081 = AXIS2_PLACEMENT_3D ( 'NONE', #528, #9695, #8711 ) ;
#10082 = CARTESIAN_POINT ( 'NONE',  ( -26.49999999999971578, -45.89934640057541060, 8.000000000000000000 ) ) ;
#10083 = DIRECTION ( 'NONE',  ( -0.000000000000000000, -0.000000000000000000, 1.000000000000000000 ) ) ;
#10084 = ORIENTED_EDGE ( 'NONE', *, *, #8388, .T. ) ;
#10085 = LINE ( 'NONE', #7657, #14302 ) ;
#10086 = ORIENTED_EDGE ( 'NONE', *, *, #12062, .F. ) ;
#10087 = ORIENTED_EDGE ( 'NONE', *, *, #8096, .F. ) ;
#10088 = FACE_OUTER_BOUND ( 'NONE', #34, .T. ) ;
#10089 = CIRCLE ( 'NONE', #11564, 3.000000000000002665 ) ;
#10090 = PLANE ( 'NONE',  #18 ) ;
#10091 = EDGE_CURVE ( 'NONE', #9453, #8412, #1948, .T. ) ;
#10092 = EDGE_CURVE ( 'NONE', #4050, #3015, #11786, .T. ) ;
#10093 = EDGE_CURVE ( 'NONE', #8421, #6180, #5844, .T. ) ;
#10094 = CARTESIAN_POINT ( 'NONE',  ( 2.449293598294700991E-16, -97.00000000000000000, 10.49999999999999822 ) ) ;
#10095 = CARTESIAN_POINT ( 'NONE',  ( 71.53347797788771345, 69.16568774265620334, -13.00000000000000178 ) ) ;
#10096 = DIRECTION ( 'NONE',  ( 0.000000000000000000, 0.000000000000000000, 1.000000000000000000 ) ) ;
#10097 = ADVANCED_FACE ( 'NONE', ( #2290 ), #80, .T. ) ;
#10098 = VERTEX_POINT ( 'NONE', #1745 ) ;
#10099 = VECTOR ( 'NONE', #3217, 1000.000000000000000 ) ;
#10100 = DIRECTION ( 'NONE',  ( 1.000000000000000000, 0.000000000000000000, 0.000000000000000000 ) ) ;
#10101 = PRODUCT_DEFINITION_SHAPE ( 'NONE', 'NONE',  #15044 ) ;
#10102 = EDGE_CURVE ( 'NONE', #8421, #7767, #1224, .T. ) ;
#10103 = CARTESIAN_POINT ( 'NONE',  ( -12.86891638962156215, 56.43380494353993271, 10.49999999999999822 ) ) ;
#10104 = DIRECTION ( 'NONE',  ( 1.000000000000000000, 0.000000000000000000, 0.000000000000000000 ) ) ;
#10105 = VERTEX_POINT ( 'NONE', #4869 ) ;
#10106 = CARTESIAN_POINT ( 'NONE',  ( 34.44830544488820578, 94.94374256356071839, -16.00000000000000000 ) ) ;
#10107 = CARTESIAN_POINT ( 'NONE',  ( 0.000000000000000000, 0.000000000000000000, -26.00000000000000000 ) ) ;
#10108 = ORIENTED_EDGE ( 'NONE', *, *, #13306, .T. ) ;
#10109 = CARTESIAN_POINT ( 'NONE',  ( -11.62509980388830577, 61.91833518448029849, 17.84018927347701933 ) ) ;
#10110 = EDGE_CURVE ( 'NONE', #1622, #1196, #2675, .T. ) ;
#10111 = CARTESIAN_POINT ( 'NONE',  ( -8.075974454121990220, 94.65787058575050139, -19.99999999999999289 ) ) ;
#10112 = CARTESIAN_POINT ( 'NONE',  ( -1.393927851585479605, 4.043713361053526079, -3.526374918436835149 ) ) ;
#10113 = FACE_OUTER_BOUND ( 'NONE', #2252, .T. ) ;
#10114 = CARTESIAN_POINT ( 'NONE',  ( 52.54657765281197612, -6.917888187662545540, -13.00000000000000178 ) ) ;
#10115 = CARTESIAN_POINT ( 'NONE',  ( -15.11621636258860946, 32.12188890498260463, 11.00000000000000000 ) ) ;
#10116 = CARTESIAN_POINT ( 'NONE',  ( 9.714003807514266953, 53.63365512954683112, 8.000000000000000000 ) ) ;
#10117 = VERTEX_POINT ( 'NONE', #13142 ) ;
#10118 = CARTESIAN_POINT ( 'NONE',  ( -68.58935777509427112, 68.58935777509594800, 8.000000000000000000 ) ) ;
#10119 = CARTESIAN_POINT ( 'NONE',  ( 10.88232432232082125, 94.37491168429329491, -18.69329470938989957 ) ) ;
#10120 = DIRECTION ( 'NONE',  ( -1.000000000000000000, 0.000000000000000000, 0.000000000000000000 ) ) ;
#10121 = CYLINDRICAL_SURFACE ( 'NONE', #5206, 63.00000000000000000 ) ;
#10122 = ORIENTED_EDGE ( 'NONE', *, *, #7217, .F. ) ;
#10123 = CARTESIAN_POINT ( 'NONE',  ( -32.26435573746199736, 42.04772703543562073, -10.50000000000000000 ) ) ;
#10124 = ORIENTED_EDGE ( 'NONE', *, *, #14358, .F. ) ;
#10125 = DIRECTION ( 'NONE',  ( 0.000000000000000000, 0.000000000000000000, -1.000000000000000000 ) ) ;
#10126 = CARTESIAN_POINT ( 'NONE',  ( 7.500000000000000000, 74.62405778299650194, 20.00000000000000000 ) ) ;
#10127 = ORIENTED_EDGE ( 'NONE', *, *, #5862, .F. ) ;
#10128 = VECTOR ( 'NONE', #4550, 1000.000000000000000 ) ;
#10129 = LINE ( 'NONE', #2010, #11676 ) ;
#10130 = DIRECTION ( 'NONE',  ( -1.000000000000000000, 0.000000000000000000, 0.000000000000000000 ) ) ;
#10131 = CONTEXT_DEPENDENT_SHAPE_REPRESENTATION ( #6863, #1612 ) ;
#10132 = ORIENTED_EDGE ( 'NONE', *, *, #10093, .T. ) ;
#10133 = ORIENTED_EDGE ( 'NONE', *, *, #2111, .F. ) ;
#10134 = ORIENTED_EDGE ( 'NONE', *, *, #10073, .F. ) ;
#10135 = EDGE_CURVE ( 'NONE', #10220, #12354, #14310, .T. ) ;
#10136 = CARTESIAN_POINT ( 'NONE',  ( 0.000000000000000000, 4.862606272033088928, -3.745885042887437510 ) ) ;
#10137 = CARTESIAN_POINT ( 'NONE',  ( 36.08010649850015739, 100.2464683348682541, 16.00000000000000000 ) ) ;
#10138 = DIRECTION ( 'NONE',  ( 1.000000000000000000, 0.000000000000000000, 0.000000000000000000 ) ) ;
#10139 = VERTEX_POINT ( 'NONE', #14210 ) ;
#10140 = ORIENTED_EDGE ( 'NONE', *, *, #10285, .F. ) ;
#10141 = ORIENTED_EDGE ( 'NONE', *, *, #2021, .F. ) ;
#10142 = CARTESIAN_POINT ( 'NONE',  ( -12.46631608856921325, 100.2277185551817809, 15.67011936326128563 ) ) ;
#10143 = VECTOR ( 'NONE', #1081, 1000.000000000000227 ) ;
#10144 = DIRECTION ( 'NONE',  ( 1.000000000000000000, 0.000000000000000000, 0.000000000000000000 ) ) ;
#10145 = DIRECTION ( 'NONE',  ( 0.000000000000000000, 1.000000000000000000, -1.471414886128460880E-15 ) ) ;
#10146 = FACE_OUTER_BOUND ( 'NONE', #10633, .T. ) ;
#10147 = DIRECTION ( 'NONE',  ( 0.000000000000000000, 0.000000000000000000, 1.000000000000000000 ) ) ;
#10148 = CARTESIAN_POINT ( 'NONE',  ( -41.94820822869193222, -33.29654390035832279, -10.50000000000000000 ) ) ;
#10149 = ORIENTED_EDGE ( 'NONE', *, *, #4079, .F. ) ;
#10150 = EDGE_CURVE ( 'NONE', #5988, #9656, #6291, .T. ) ;
#10151 = EDGE_CURVE ( 'NONE', #6653, #5203, #453, .T. ) ;
#10152 = CARTESIAN_POINT ( 'NONE',  ( -2.449293598294700991E-16, 97.00000000000000000, -10.50000000000000000 ) ) ;
#10153 = VERTEX_POINT ( 'NONE', #9775 ) ;
#10154 = ORIENTED_EDGE ( 'NONE', *, *, #13980, .T. ) ;
#10155 = FACE_OUTER_BOUND ( 'NONE', #13085, .T. ) ;
#10156 = CARTESIAN_POINT ( 'NONE',  ( -52.54657765281192638, 6.917888187662934563, -10.50000000000000000 ) ) ;
#10157 = AXIS2_PLACEMENT_3D ( 'NONE', #9486, #3885, #9632 ) ;
#10158 = CARTESIAN_POINT ( 'NONE',  ( -26.49999999999971578, -45.89934640057541060, -10.50000000000000000 ) ) ;
#10159 = ORIENTED_EDGE ( 'NONE', *, *, #5931, .F. ) ;
#10160 = CARTESIAN_POINT ( 'NONE',  ( -36.24943435566822103, 100.7967187407115262, -10.99999999999999645 ) ) ;
#10161 = DIRECTION ( 'NONE',  ( -0.000000000000000000, -0.000000000000000000, 1.000000000000000000 ) ) ;
#10162 = DIRECTION ( 'NONE',  ( -1.000000000000000000, 0.000000000000000000, 0.000000000000000000 ) ) ;
#10163 = ORIENTED_EDGE ( 'NONE', *, *, #5316, .F. ) ;
#10164 = AXIS2_PLACEMENT_3D ( 'NONE', #2782, #11059, #13323 ) ;
#10165 = CARTESIAN_POINT ( 'NONE',  ( 2.500000000000002220, -2.357898499370437939, 0.000000000000000000 ) ) ;
#10166 = ORIENTED_EDGE ( 'NONE', *, *, #8469, .T. ) ;
#10167 = DIRECTION ( 'NONE',  ( 0.000000000000000000, 0.000000000000000000, 1.000000000000000000 ) ) ;
#10168 = AXIS2_PLACEMENT_3D ( 'NONE', #3497, #11624, #10471 ) ;
#10169 = CARTESIAN_POINT ( 'NONE',  ( -96.58511096861892042, -0.2790467552922097916, 10.49999999999999822 ) ) ;
#10170 = ADVANCED_FACE ( 'NONE', ( #13220 ), #14427, .T. ) ;
#10171 = ORIENTED_EDGE ( 'NONE', *, *, #733, .T. ) ;
#10172 = CARTESIAN_POINT ( 'NONE',  ( 9.706953719245472456, 57.06275842387054098, -13.00000000000000178 ) ) ;
#10173 = ORIENTED_EDGE ( 'NONE', *, *, #3242, .F. ) ;
#10174 = CARTESIAN_POINT ( 'NONE',  ( 33.22084910410213610, 95.38070844757928057, 15.83879782491088761 ) ) ;
#10175 = ADVANCED_FACE ( 'NONE', ( #5162 ), #7354, .T. ) ;
#10176 = DIRECTION ( 'NONE',  ( 1.000000000000000000, 0.000000000000000000, 0.000000000000000000 ) ) ;
#10177 = AXIS2_PLACEMENT_3D ( 'NONE', #1621, #4052, #14519 ) ;
#10178 = CARTESIAN_POINT ( 'NONE',  ( -9.719110480984905820, 94.50309565249440880, -19.51732164073033715 ) ) ;
#10180 = DIRECTION ( 'NONE',  ( 0.000000000000000000, 0.000000000000000000, 1.000000000000000000 ) ) ;
#10179 = VECTOR ( 'NONE', #6627, 1000.000000000000000 ) ;
#10181 = DIRECTION ( 'NONE',  ( 0.000000000000000000, 0.000000000000000000, 1.000000000000000000 ) ) ;
#10182 = EDGE_CURVE ( 'NONE', #9719, #13003, #3735, .T. ) ;
#10183 = AXIS2_PLACEMENT_3D ( 'NONE', #2377, #3533, #178 ) ;
#10184 = CYLINDRICAL_SURFACE ( 'NONE', #5070, 3.000000000000002665 ) ;
#10186 = PLANE ( 'NONE',  #8577 ) ;
#10185 = VECTOR ( 'NONE', #1306, 1000.000000000000000 ) ;
#10187 = ORIENTED_EDGE ( 'NONE', *, *, #6012, .T. ) ;
#10188 = CARTESIAN_POINT ( 'NONE',  ( -53.63365512954686665, 9.714003807514082212, -13.00000000000000178 ) ) ;
#10189 = CYLINDRICAL_SURFACE ( 'NONE', #6145, 0.5000000000000004441 ) ;
#10190 = EDGE_CURVE ( 'NONE', #9586, #11551, #8251, .T. ) ;
#10191 = AXIS2_PLACEMENT_3D ( 'NONE', #1525, #1602, #8426 ) ;
#10192 = EDGE_CURVE ( 'NONE', #12171, #8537, #13339, .T. ) ;
#10193 = CARTESIAN_POINT ( 'NONE',  ( 41.59008834022645829, 32.46576781417968505, -10.50000000000000000 ) ) ;
#10194 = CIRCLE ( 'NONE', #7515, 3.000000000000002665 ) ;
#10195 = CARTESIAN_POINT ( 'NONE',  ( 0.000000000000000000, 0.000000000000000000, -8.000000000000000000 ) ) ;
#10196 = VECTOR ( 'NONE', #1433, 1000.000000000000000 ) ;
#10197 = ORIENTED_EDGE ( 'NONE', *, *, #5708, .F. ) ;
#10198 = DIRECTION ( 'NONE',  ( 0.2941176470588243164, 0.9557692240748185686, -0.000000000000000000 ) ) ;
#10199 = ORIENTED_EDGE ( 'NONE', *, *, #12185, .F. ) ;
#10200 = CYLINDRICAL_SURFACE ( 'NONE', #3281, 2.500000000000000444 ) ;
#10201 = DIRECTION ( 'NONE',  ( -1.000000000000000000, 0.000000000000000000, 0.000000000000000000 ) ) ;
#10202 = EDGE_CURVE ( 'NONE', #1809, #5665, #10076, .T. ) ;
#10203 = AXIS2_PLACEMENT_3D ( 'NONE', #1594, #379, #10918 ) ;
#10204 = ORIENTED_EDGE ( 'NONE', *, *, #3771, .T. ) ;
#10205 = AXIS2_PLACEMENT_3D ( 'NONE', #8874, #13508, #11240 ) ;
#10206 = CARTESIAN_POINT ( 'NONE',  ( -52.54657765281192638, 6.917888187662934563, -13.00000000000000178 ) ) ;
#10207 = DIRECTION ( 'NONE',  ( 0.000000000000000000, 0.000000000000000000, -1.000000000000000000 ) ) ;
#10208 = APPLICATION_PROTOCOL_DEFINITION ( 'draft international standard', 'automotive_design', 1998, #5439 ) ;
#10209 = ORIENTED_EDGE ( 'NONE', *, *, #1930, .T. ) ;
#10210 = CIRCLE ( 'NONE', #11926, 0.5000000000000004441 ) ;
#10211 = ORIENTED_EDGE ( 'NONE', *, *, #3291, .T. ) ;
#10212 = ORIENTED_EDGE ( 'NONE', *, *, #14090, .F. ) ;
#10213 = VERTEX_POINT ( 'NONE', #2879 ) ;
#10214 = DIRECTION ( 'NONE',  ( 0.000000000000000000, 0.000000000000000000, -1.000000000000000000 ) ) ;
#10215 = DIRECTION ( 'NONE',  ( 0.000000000000000000, 0.000000000000000000, 1.000000000000000000 ) ) ;
#10216 = CARTESIAN_POINT ( 'NONE',  ( 25.00000000000000000, 81.24038404635960831, -13.50000000000000178 ) ) ;
#10217 = ORIENTED_EDGE ( 'NONE', *, *, #1066, .T. ) ;
#10218 = AXIS2_PLACEMENT_3D ( 'NONE', #7454, #1351, #14456 ) ;
#10219 = ORIENTED_EDGE ( 'NONE', *, *, #5242, .F. ) ;
#10220 = VERTEX_POINT ( 'NONE', #12151 ) ;
#10221 = AXIS2_PLACEMENT_3D ( 'NONE', #5646, #14922, #12562 ) ;
#10222 = CARTESIAN_POINT ( 'NONE',  ( 12.34196858416779996, 73.97755844198597686, 16.27929523640516862 ) ) ;
#10223 = CARTESIAN_POINT ( 'NONE',  ( 0.000000000000000000, 0.000000000000000000, -13.00000000000000178 ) ) ;
#10224 = DIRECTION ( 'NONE',  ( 1.000000000000000000, 0.000000000000000000, 0.000000000000000000 ) ) ;
#10225 = FILL_AREA_STYLE_COLOUR ( '', #11142 ) ;
#10226 = FACE_OUTER_BOUND ( 'NONE', #13181, .T. ) ;
#10227 = VECTOR ( 'NONE', #8208, 1000.000000000000000 ) ;
#10228 = DIRECTION ( 'NONE',  ( -0.000000000000000000, -0.000000000000000000, 1.000000000000000000 ) ) ;
#10229 = EDGE_LOOP ( 'NONE', ( #5736, #1795, #5434, #11964, #11756 ) ) ;
#10230 = VERTEX_POINT ( 'NONE', #227 ) ;
#10231 = CARTESIAN_POINT ( 'NONE',  ( -26.49999999999971578, -45.89934640057541060, -8.000000000000000000 ) ) ;
#10232 = ORIENTED_EDGE ( 'NONE', *, *, #7202, .F. ) ;
#10233 = VECTOR ( 'NONE', #10054, 1000.000000000000114 ) ;
#10234 = ORIENTED_EDGE ( 'NONE', *, *, #10451, .T. ) ;
#10235 = ORIENTED_EDGE ( 'NONE', *, *, #7437, .F. ) ;
#10236 = DIRECTION ( 'NONE',  ( -1.000000000000000000, 0.000000000000000000, 0.000000000000000000 ) ) ;
#10237 = EDGE_CURVE ( 'NONE', #4479, #13246, #7726, .T. ) ;
#10238 = CIRCLE ( 'NONE', #9504, 0.5000000000000004441 ) ;
#10239 = EDGE_CURVE ( 'NONE', #12645, #7413, #7577, .T. ) ;
#10240 = ORIENTED_EDGE ( 'NONE', *, *, #8851, .T. ) ;
#10241 = ADVANCED_FACE ( 'NONE', ( #3042 ), #14499, .F. ) ;
#10242 = EDGE_CURVE ( 'NONE', #12545, #13279, #4136, .T. ) ;
#10243 = FACE_OUTER_BOUND ( 'NONE', #8199, .T. ) ;
#10244 = CARTESIAN_POINT ( 'NONE',  ( 9.706953719245472456, 57.06275842387054098, -13.00000000000000178 ) ) ;
#10245 = ORIENTED_EDGE ( 'NONE', *, *, #3993, .T. ) ;
#10246 = VECTOR ( 'NONE', #2901, 1000.000000000000000 ) ;
#10247 = PLANE ( 'NONE',  #1345 ) ;
#10248 = CARTESIAN_POINT ( 'NONE',  ( -0.5276280594147905179, 4.314175951381877816, -3.320322319202512418 ) ) ;
#10249 = CARTESIAN_POINT ( 'NONE',  ( 71.58935777509475429, -68.58935777509547904, -13.00000000000000178 ) ) ;
#10250 = ORIENTED_EDGE ( 'NONE', *, *, #5483, .T. ) ;
#10251 = FACE_OUTER_BOUND ( 'NONE', #5004, .T. ) ;
#10252 = CIRCLE ( 'NONE', #3221, 10.00000000000000355 ) ;
#10253 = CARTESIAN_POINT ( 'NONE',  ( -97.41488903138106537, 0.2790467552942557661, -10.50000000000000000 ) ) ;
#10254 = CARTESIAN_POINT ( 'NONE',  ( -20.00000000000000000, 2.449293598294706513E-15, -43.49999999999998579 ) ) ;
#10255 = CIRCLE ( 'NONE', #2263, 53.55662432702593634 ) ;
#10256 = ORIENTED_EDGE ( 'NONE', *, *, #14604, .F. ) ;
#10257 = ADVANCED_FACE ( 'NONE', ( #14583 ), #4186, .F. ) ;
#10258 = CARTESIAN_POINT ( 'NONE',  ( -97.00000000000000000, 1.015776140243522349E-12, 10.49999999999999822 ) ) ;
#10259 = CIRCLE ( 'NONE', #13415, 4.000000000000000000 ) ;
#10260 = CARTESIAN_POINT ( 'NONE',  ( -51.19406879332065330, -13.71740939043347041, -13.00000000000000178 ) ) ;
#10261 = EDGE_CURVE ( 'NONE', #10098, #5511, #1462, .T. ) ;
#10262 = DIRECTION ( 'NONE',  ( 1.000000000000000000, 0.000000000000000000, 0.000000000000000000 ) ) ;
#10263 = VECTOR ( 'NONE', #9606, 1000.000000000000000 ) ;
#10264 = CARTESIAN_POINT ( 'NONE',  ( -10.21436410913239357, 94.45034564433045432, -19.23824501837257017 ) ) ;
#10265 = LINE ( 'NONE', #6978, #261 ) ;
#10266 = DIRECTION ( 'NONE',  ( -0.9557692240748187906, -0.2941176470588238168, 0.000000000000000000 ) ) ;
#10267 = DIRECTION ( 'NONE',  ( -0.000000000000000000, -0.000000000000000000, 1.000000000000000000 ) ) ;
#10268 = CYLINDRICAL_SURFACE ( 'NONE', #2517, 5.000000000000000888 ) ;
#10269 = DIRECTION ( 'NONE',  ( 1.000000000000000000, 0.000000000000000000, 0.000000000000000000 ) ) ;
#10270 = CONICAL_SURFACE ( 'NONE', #7098, 55.00000000000000000, 0.5235987755983000369 ) ;
#10271 = ORIENTED_EDGE ( 'NONE', *, *, #9138, .T. ) ;
#10272 = DIRECTION ( 'NONE',  ( 1.000000000000000000, 0.000000000000000000, 0.000000000000000000 ) ) ;
#10273 = DIRECTION ( 'NONE',  ( 0.000000000000000000, 0.000000000000000000, 1.000000000000000000 ) ) ;
#10274 = CIRCLE ( 'NONE', #6371, 4.000000000000000000 ) ;
#10275 = CARTESIAN_POINT ( 'NONE',  ( 3.999999999999996447, -2.309401076758518911, -3.433295621305385126 ) ) ;
#10276 = CARTESIAN_POINT ( 'NONE',  ( 26.49999999999971578, 45.89934640057541060, -8.000000000000000000 ) ) ;
#10277 = ORIENTED_EDGE ( 'NONE', *, *, #5225, .F. ) ;
#10278 = DIRECTION ( 'NONE',  ( -0.000000000000000000, -0.000000000000000000, 1.000000000000000000 ) ) ;
#10279 = AXIS2_PLACEMENT_3D ( 'NONE', #6461, #7755, #11265 ) ;
#10280 = EDGE_LOOP ( 'NONE', ( #860, #3397, #5194, #3581 ) ) ;
#10281 = FACE_OUTER_BOUND ( 'NONE', #11906, .T. ) ;
#10282 = DIRECTION ( 'NONE',  ( -1.000000000000000000, 0.000000000000000000, 0.000000000000000000 ) ) ;
#10283 = EDGE_CURVE ( 'NONE', #6334, #1631, #10679, .T. ) ;
#10284 = CARTESIAN_POINT ( 'NONE',  ( 7.500000000000000888, 106.7368258849775202, -20.00000000000000000 ) ) ;
#10285 = EDGE_CURVE ( 'NONE', #5509, #8172, #6064, .T. ) ;
#10286 = CARTESIAN_POINT ( 'NONE',  ( -42.50536573064432133, -32.06294366074479996, 10.49999999999999822 ) ) ;
#10287 = VERTEX_POINT ( 'NONE', #917 ) ;
#10288 = ADVANCED_FACE ( 'NONE', ( #3113 ), #1967, .F. ) ;
#10289 = ORIENTED_EDGE ( 'NONE', *, *, #3098, .F. ) ;
#10290 = VECTOR ( 'NONE', #3851, 1000.000000000000000 ) ;
#10291 = CYLINDRICAL_SURFACE ( 'NONE', #7418, 0.5000000000000004441 ) ;
#10292 = CARTESIAN_POINT ( 'NONE',  ( 35.08068705722487124, 100.7955773171491813, 15.87635720896652458 ) ) ;
#10293 = LINE ( 'NONE', #2385, #8781 ) ;
#10294 = VERTEX_POINT ( 'NONE', #1892 ) ;
#10295 = ADVANCED_FACE ( 'NONE', ( #843 ), #8714, .T. ) ;
#10296 = ORIENTED_EDGE ( 'NONE', *, *, #10013, .F. ) ;
#10297 = CIRCLE ( 'NONE', #11533, 3.000000000000002665 ) ;
#10298 = ORIENTED_EDGE ( 'NONE', *, *, #3477, .F. ) ;
#10299 = AXIS2_PLACEMENT_3D ( 'NONE', #6702, #3152, #885 ) ;
#10300 = CARTESIAN_POINT ( 'NONE',  ( -12.50000000000000000, 59.24038404635959409, 20.00000000000000000 ) ) ;
#10301 = AXIS2_PLACEMENT_3D ( 'NONE', #228, #84, #8278 ) ;
#10302 = DIRECTION ( 'NONE',  ( -1.000000000000000000, 0.000000000000000000, 0.000000000000000000 ) ) ;
#10303 = ADVANCED_FACE ( 'NONE', ( #13359 ), #10090, .F. ) ;
#10304 = CARTESIAN_POINT ( 'NONE',  ( -22.33583958711380646, -30.74264578624812927, -28.00000000000000000 ) ) ;
#10305 = DIRECTION ( 'NONE',  ( 0.000000000000000000, 0.000000000000000000, -1.000000000000000000 ) ) ;
#10306 = ORIENTED_EDGE ( 'NONE', *, *, #2398, .T. ) ;
#10307 = DIRECTION ( 'NONE',  ( 1.000000000000000000, 0.000000000000000000, 0.000000000000000000 ) ) ;
#10308 = ORIENTED_EDGE ( 'NONE', *, *, #11567, .F. ) ;
#10309 = EDGE_LOOP ( 'NONE', ( #7104, #5284, #4095, #519 ) ) ;
#10310 = LINE ( 'NONE', #2180, #4730 ) ;
#10311 = CYLINDRICAL_SURFACE ( 'NONE', #12557, 4.250000000000000000 ) ;
#10312 = AXIS2_PLACEMENT_3D ( 'NONE', #13912, #3507, #8126 ) ;
#10313 = ORIENTED_EDGE ( 'NONE', *, *, #9060, .F. ) ;
#10314 = AXIS2_PLACEMENT_3D ( 'NONE', #11698, #3494, #8186 ) ;
#10315 = VERTEX_POINT ( 'NONE', #4334 ) ;
#10316 = DIRECTION ( 'NONE',  ( -1.000000000000000000, 0.000000000000000000, 0.000000000000000000 ) ) ;
#10317 = EDGE_LOOP ( 'NONE', ( #9010, #6395, #8933, #11522 ) ) ;
#10318 = ORIENTED_EDGE ( 'NONE', *, *, #3161, .F. ) ;
#10319 = VECTOR ( 'NONE', #13553, 1000.000000000000000 ) ;
#10320 = DIRECTION ( 'NONE',  ( 0.2941176470588243164, 0.9557692240748185686, 0.000000000000000000 ) ) ;
#10321 = DIRECTION ( 'NONE',  ( 0.000000000000000000, 0.000000000000000000, -1.000000000000000000 ) ) ;
#10322 = CIRCLE ( 'NONE', #1833, 75.00000000000001421 ) ;
#10323 = DIRECTION ( 'NONE',  ( 0.9396926207859138680, 1.150791560227856926E-16, -0.3420201433256536139 ) ) ;
#10324 = CARTESIAN_POINT ( 'NONE',  ( 89.61631465359468507, -37.12029293941410657, -13.00000000000000178 ) ) ;
#10325 = CYLINDRICAL_SURFACE ( 'NONE', #12608, 0.5000000000000022204 ) ;
#10326 = ORIENTED_EDGE ( 'NONE', *, *, #5517, .F. ) ;
#10327 = CARTESIAN_POINT ( 'NONE',  ( -100.0000000000000000, 0.000000000000000000, 13.00000000000000178 ) ) ;
#10328 = EDGE_CURVE ( 'NONE', #12813, #14403, #2046, .T. ) ;
#10329 = CIRCLE ( 'NONE', #14216, 20.00000000000000000 ) ;
#10330 = CARTESIAN_POINT ( 'NONE',  ( -6.917888187662729393, -52.54657765281195481, -8.000000000000000000 ) ) ;
#10331 = CARTESIAN_POINT ( 'NONE',  ( -4.198928548860770604, 0.8158838809860071706, -3.526471437616916837 ) ) ;
#10332 = EDGE_CURVE ( 'NONE', #13279, #3803, #5354, .T. ) ;
#10333 = VERTEX_POINT ( 'NONE', #5536 ) ;
#10334 = CARTESIAN_POINT ( 'NONE',  ( 56.43380494353997534, 12.86891638962136319, -13.00000000000000178 ) ) ;
#10335 = ORIENTED_EDGE ( 'NONE', *, *, #275, .F. ) ;
#10336 = CARTESIAN_POINT ( 'NONE',  ( 3.999999999999996447, 2.309401076758511806, -0.5000000000000004441 ) ) ;
#10337 = DIRECTION ( 'NONE',  ( 0.000000000000000000, -0.5000000000000008882, -0.8660254037844380415 ) ) ;
#10338 = CARTESIAN_POINT ( 'NONE',  ( 47.21331623427115431, 33.48561063518610581, -8.000000000000000000 ) ) ;
#10339 = CARTESIAN_POINT ( 'NONE',  ( -12.50000000000000000, 106.2673515243510991, 15.00000000000000000 ) ) ;
#10340 = CYLINDRICAL_SURFACE ( 'NONE', #5403, 10.00000000000000178 ) ;
#10341 = AXIS2_PLACEMENT_3D ( 'NONE', #1169, #2228, #945 ) ;
#10342 = CARTESIAN_POINT ( 'NONE',  ( -4.211405944401396262, -2.460460786169389014, -3.751298493805494960 ) ) ;
#10343 = ADVANCED_FACE ( 'NONE', ( #2958 ), #8731, .F. ) ;
#10344 = DIRECTION ( 'NONE',  ( -1.000000000000000000, -1.765157221169382931E-15, 0.000000000000000000 ) ) ;
#10345 = ORIENTED_EDGE ( 'NONE', *, *, #10472, .T. ) ;
#10346 = EDGE_CURVE ( 'NONE', #13523, #6738, #4411, .T. ) ;
#10347 = EDGE_CURVE ( 'NONE', #9024, #11429, #3669, .T. ) ;
#10348 = CARTESIAN_POINT ( 'NONE',  ( 70.20695371924547601, 57.06275842387054098, -13.00000000000000178 ) ) ;
#10349 = FACE_OUTER_BOUND ( 'NONE', #8533, .T. ) ;
#10350 = DIRECTION ( 'NONE',  ( -0.9557692240748187906, 0.2941176470588240388, 0.000000000000000000 ) ) ;
#10351 = AXIS2_PLACEMENT_3D ( 'NONE', #542, #773, #5171 ) ;
#10352 = DIRECTION ( 'NONE',  ( -0.000000000000000000, -0.000000000000000000, 1.000000000000000000 ) ) ;
#10353 = ORIENTED_EDGE ( 'NONE', *, *, #12062, .T. ) ;
#10354 = CYLINDRICAL_SURFACE ( 'NONE', #10697, 56.99999999999999289 ) ;
#10355 = VERTEX_POINT ( 'NONE', #4628 ) ;
#10356 = FACE_OUTER_BOUND ( 'NONE', #2558, .T. ) ;
#10357 = CARTESIAN_POINT ( 'NONE',  ( -45.89934640057513349, 26.50000000000019540, -10.50000000000000000 ) ) ;
#10358 = DIRECTION ( 'NONE',  ( -0.000000000000000000, -0.000000000000000000, -1.000000000000000000 ) ) ;
#10359 = DIRECTION ( 'NONE',  ( -1.000000000000000000, -1.776356839400250465E-15, 0.000000000000000000 ) ) ;
#10360 = ORIENTED_EDGE ( 'NONE', *, *, #6039, .F. ) ;
#10361 = ORIENTED_EDGE ( 'NONE', *, *, #8217, .F. ) ;
#10362 = VERTEX_POINT ( 'NONE', #14037 ) ;
#10363 = FACE_OUTER_BOUND ( 'NONE', #12554, .T. ) ;
#10364 = CARTESIAN_POINT ( 'NONE',  ( 68.58935777509475429, -68.58935777509547904, -13.00000000000000178 ) ) ;
#10365 = DIRECTION ( 'NONE',  ( 0.000000000000000000, 0.000000000000000000, 1.000000000000000000 ) ) ;
#10366 = ORIENTED_EDGE ( 'NONE', *, *, #9036, .T. ) ;
#10367 = ADVANCED_FACE ( 'NONE', ( #10465 ), #11471, .T. ) ;
#10368 = ADVANCED_FACE ( 'NONE', ( #6960, #12755 ), #1208, .T. ) ;
#10369 = EDGE_CURVE ( 'NONE', #7243, #10452, #13748, .T. ) ;
#10370 = ORIENTED_EDGE ( 'NONE', *, *, #13933, .F. ) ;
#10371 = EDGE_LOOP ( 'NONE', ( #13790, #10904, #5745, #13778 ) ) ;
#10372 = ADVANCED_FACE ( 'NONE', ( #4705 ), #3336, .T. ) ;
#10373 = CARTESIAN_POINT ( 'NONE',  ( 0.000000000000000000, 0.000000000000000000, -28.00000000000000000 ) ) ;
#10374 = DIRECTION ( 'NONE',  ( 1.000000000000000000, 0.000000000000000000, 0.000000000000000000 ) ) ;
#10375 = DIRECTION ( 'NONE',  ( -0.000000000000000000, 1.000000000000000000, -0.000000000000000000 ) ) ;
#10376 = SURFACE_STYLE_USAGE ( .BOTH. , #9302 ) ;
#10377 = DIRECTION ( 'NONE',  ( 0.000000000000000000, 0.000000000000000000, 1.000000000000000000 ) ) ;
#10378 = EDGE_CURVE ( 'NONE', #14446, #4759, #7038, .T. ) ;
#10379 = ORIENTED_EDGE ( 'NONE', *, *, #14648, .F. ) ;
#10380 = CARTESIAN_POINT ( 'NONE',  ( 4.000000000000000000, -2.309401076758517135, -3.504271511727127475 ) ) ;
#10381 = EDGE_LOOP ( 'NONE', ( #868, #3319, #13158, #14558, #8424 ) ) ;
#10382 = VERTEX_POINT ( 'NONE', #13974 ) ;
#10383 = CARTESIAN_POINT ( 'NONE',  ( -29.26435573746199381, 42.04772703543562073, -13.00000000000000178 ) ) ;
#10384 = CARTESIAN_POINT ( 'NONE',  ( 20.00000000000000000, 64.99230723708768664, 31.00000000000000000 ) ) ;
#10385 = ORIENTED_EDGE ( 'NONE', *, *, #686, .T. ) ;
#10386 = EDGE_CURVE ( 'NONE', #1155, #8687, #7954, .T. ) ;
#10387 = ADVANCED_FACE ( 'NONE', ( #10243 ), #5607, .F. ) ;
#10388 = ORIENTED_EDGE ( 'NONE', *, *, #5009, .F. ) ;
#10389 = DIRECTION ( 'NONE',  ( -1.000000000000000000, 0.000000000000000000, 0.000000000000000000 ) ) ;
#10390 = ORIENTED_EDGE ( 'NONE', *, *, #2040, .T. ) ;
#10391 = VERTEX_POINT ( 'NONE', #12821 ) ;
#10392 = DIRECTION ( 'NONE',  ( -1.000000000000000000, 0.000000000000000000, 0.000000000000000000 ) ) ;
#10393 = DIRECTION ( 'NONE',  ( -1.000000000000000000, 0.000000000000000000, 0.000000000000000000 ) ) ;
#10394 = CARTESIAN_POINT ( 'NONE',  ( -1.655952806101423258, 3.662737355149033203, 1.383628319339899209E-15 ) ) ;
#10395 = DIRECTION ( 'NONE',  ( 1.000000000000000000, 0.000000000000000000, -0.000000000000000000 ) ) ;
#10396 = VERTEX_POINT ( 'NONE', #1145 ) ;
#10397 = DIRECTION ( 'NONE',  ( -1.000000000000000000, 0.000000000000000000, 0.000000000000000000 ) ) ;
#10398 = ORIENTED_EDGE ( 'NONE', *, *, #7477, .F. ) ;
#10399 = DIRECTION ( 'NONE',  ( 0.000000000000000000, 0.000000000000000000, 1.000000000000000000 ) ) ;
#10400 = CARTESIAN_POINT ( 'NONE',  ( -89.12622059913283579, -37.21932736666236963, -13.00000000000000178 ) ) ;
#10401 = ORIENTED_EDGE ( 'NONE', *, *, #11282, .T. ) ;
#10402 = FACE_OUTER_BOUND ( 'NONE', #11531, .T. ) ;
#10403 = AXIS2_PLACEMENT_3D ( 'NONE', #14435, #8501, #2883 ) ;
#10404 = DIRECTION ( 'NONE',  ( 0.000000000000000000, 0.000000000000000000, 1.000000000000000000 ) ) ;
#10405 = B_SPLINE_CURVE_WITH_KNOTS ( 'NONE', 3,
 ( #11045, #4133, #4062, #12105, #11116, #6536, #13390, #14459, #8901, #8750 ),
 .UNSPECIFIED., .F., .F.,
 ( 4, 2, 2, 2, 4 ),
 ( 0.000000000000000000, 0.001711864931188371644, 0.003423729862376743288, 0.005135594793565114932, 0.006847459724753486576 ),
 .UNSPECIFIED. ) ;
#10406 = CARTESIAN_POINT ( 'NONE',  ( -33.48561063518626923, 47.21331623427104063, 8.000000000000000000 ) ) ;
#10407 = FACE_OUTER_BOUND ( 'NONE', #7166, .T. ) ;
#10408 = DIRECTION ( 'NONE',  ( -0.000000000000000000, -0.000000000000000000, 1.000000000000000000 ) ) ;
#10409 = CARTESIAN_POINT ( 'NONE',  ( -22.33583958711380646, -30.74264578624812927, -25.50000000000000355 ) ) ;
#10410 = CARTESIAN_POINT ( 'NONE',  ( -49.00442420935969778, 30.80502811811250297, 10.49999999999999822 ) ) ;
#10411 = CIRCLE ( 'NONE', #4124, 22.00000000000001421 ) ;
#10412 = CARTESIAN_POINT ( 'NONE',  ( -57.06275842387042729, 9.706953719246069312, -8.000000000000000000 ) ) ;
#10413 = ORIENTED_EDGE ( 'NONE', *, *, #8764, .T. ) ;
#10414 = DIRECTION ( 'NONE',  ( 0.000000000000000000, 0.000000000000000000, -1.000000000000000000 ) ) ;
#10415 = CARTESIAN_POINT ( 'NONE',  ( 45.91029614918936375, -26.00011991137331790, -13.00000000000000178 ) ) ;
#10416 = DIRECTION ( 'NONE',  ( 0.000000000000000000, 0.000000000000000000, 1.000000000000000000 ) ) ;
#10417 = AXIS2_PLACEMENT_3D ( 'NONE', #8486, #13135, #3804 ) ;
#10418 = DIRECTION ( 'NONE',  ( 0.000000000000000000, 0.000000000000000000, 1.000000000000000000 ) ) ;
#10419 = ORIENTED_EDGE ( 'NONE', *, *, #3525, .T. ) ;
#10420 = CIRCLE ( 'NONE', #5330, 53.55662432702593634 ) ;
#10421 = DIRECTION ( 'NONE',  ( 1.000000000000000000, 0.000000000000000000, 0.000000000000000000 ) ) ;
#10422 = AXIS2_PLACEMENT_3D ( 'NONE', #7151, #5865, #1032 ) ;
#10423 = ORIENTED_EDGE ( 'NONE', *, *, #1088, .F. ) ;
#10424 = EDGE_CURVE ( 'NONE', #5889, #10698, #7525, .T. ) ;
#10425 = AXIS2_PLACEMENT_3D ( 'NONE', #14132, #13000, #1528 ) ;
#10426 = DIRECTION ( 'NONE',  ( -0.000000000000000000, -0.000000000000000000, -1.000000000000000000 ) ) ;
#10427 = EDGE_CURVE ( 'NONE', #11737, #7919, #12153, .T. ) ;
#10428 = CARTESIAN_POINT ( 'NONE',  ( 0.000000000000000000, 0.000000000000000000, -13.00000000000000178 ) ) ;
#10429 = EDGE_CURVE ( 'NONE', #10153, #1144, #14324, .T. ) ;
#10430 = DIRECTION ( 'NONE',  ( 0.000000000000000000, 0.000000000000000000, -1.000000000000000000 ) ) ;
#10431 = CARTESIAN_POINT ( 'NONE',  ( 0.000000000000000000, 0.000000000000000000, -10.50000000000000000 ) ) ;
#10432 = AXIS2_PLACEMENT_3D ( 'NONE', #11491, #1223, #12693 ) ;
#10433 = ORIENTED_EDGE ( 'NONE', *, *, #7731, .T. ) ;
#10434 = DIRECTION ( 'NONE',  ( 0.000000000000000000, 0.000000000000000000, -1.000000000000000000 ) ) ;
#10435 = AXIS2_PLACEMENT_3D ( 'NONE', #8203, #5770, #163 ) ;
#10436 = CARTESIAN_POINT ( 'NONE',  ( 2.500000000000002220, 1.178949249685215417, 2.042000000000002036 ) ) ;
#10437 = CARTESIAN_POINT ( 'NONE',  ( -41.59008834022669987, -32.46576781417940794, -10.50000000000000000 ) ) ;
#10438 = EDGE_LOOP ( 'NONE', ( #1835, #1245, #13913, #8165, #12497, #4132, #11726, #1149, #3821, #14184, #12096, #7999 ) ) ;
#10439 = ORIENTED_EDGE ( 'NONE', *, *, #14836, .T. ) ;
#10440 = COLOUR_RGB ( '', 0.40784314, 0.44705882, 0.49803922) ;
#10441 = ORIENTED_EDGE ( 'NONE', *, *, #3331, .T. ) ;
#10442 = CIRCLE ( 'NONE', #12389, 0.5000000000000004441 ) ;
#10443 = FACE_OUTER_BOUND ( 'NONE', #488, .T. ) ;
#10444 = CIRCLE ( 'NONE', #12877, 52.50000000000000711 ) ;
#10445 = DIRECTION ( 'NONE',  ( 1.000000000000000000, 0.000000000000000000, 0.000000000000000000 ) ) ;
#10446 = CIRCLE ( 'NONE', #13123, 56.99999999999999289 ) ;
#10447 = CARTESIAN_POINT ( 'NONE',  ( 50.00000000000000000, 6.123233995736766085E-15, 13.00000000000000178 ) ) ;
#10448 = SURFACE_SIDE_STYLE ('',( #6793 ) ) ;
#10449 = CARTESIAN_POINT ( 'NONE',  ( 30.80502811811196295, 49.00442420936003174, -10.50000000000000000 ) ) ;
#10450 = DIRECTION ( 'NONE',  ( 0.000000000000000000, 0.000000000000000000, 1.000000000000000000 ) ) ;
#10451 = EDGE_CURVE ( 'NONE', #5144, #14021, #4635, .T. ) ;
#10452 = VERTEX_POINT ( 'NONE', #14962 ) ;
#10453 = ORIENTED_EDGE ( 'NONE', *, *, #9911, .F. ) ;
#10454 = EDGE_CURVE ( 'NONE', #10950, #4578, #8036, .T. ) ;
#10455 = CARTESIAN_POINT ( 'NONE',  ( 4.211140560182194292, 2.431303136016534250, -3.745885042887433958 ) ) ;
#10456 = CARTESIAN_POINT ( 'NONE',  ( -42.89934640057513349, 26.50000000000019540, 8.000000000000000000 ) ) ;
#10457 = VECTOR ( 'NONE', #12140, 1000.000000000000000 ) ;
#10458 = ORIENTED_EDGE ( 'NONE', *, *, #9144, .F. ) ;
#10459 = AXIS2_PLACEMENT_3D ( 'NONE', #10646, #13862, #8155 ) ;
#10460 = VECTOR ( 'NONE', #3366, 1000.000000000000114 ) ;
#10461 = ORIENTED_EDGE ( 'NONE', *, *, #9437, .F. ) ;
#10462 = DIRECTION ( 'NONE',  ( -1.000000000000000000, 0.000000000000000000, 0.000000000000000000 ) ) ;
#10463 = ORIENTED_EDGE ( 'NONE', *, *, #8552, .F. ) ;
#10464 = ORIENTED_EDGE ( 'NONE', *, *, #11085, .F. ) ;
#10465 = FACE_OUTER_BOUND ( 'NONE', #6924, .T. ) ;
#10466 = CARTESIAN_POINT ( 'NONE',  ( -3.999999999999996447, 2.309401076758498039, -0.4999999999999935052 ) ) ;
#10467 = CIRCLE ( 'NONE', #6822, 56.99999999999999289 ) ;
#10468 = CARTESIAN_POINT ( 'NONE',  ( -49.00442420935969778, 30.80502811811250297, -13.00000000000000178 ) ) ;
#10469 = PLANE ( 'NONE',  #3165 ) ;
#10470 = ADVANCED_FACE ( 'NONE', ( #9172 ), #6811, .F. ) ;
#10471 = DIRECTION ( 'NONE',  ( -1.000000000000000000, 0.000000000000000000, 0.000000000000000000 ) ) ;
#10472 = EDGE_CURVE ( 'NONE', #2085, #13671, #10442, .T. ) ;
#10473 = VECTOR ( 'NONE', #9324, 1000.000000000000000 ) ;
#10474 = ORIENTED_EDGE ( 'NONE', *, *, #13785, .F. ) ;
#10475 = CYLINDRICAL_SURFACE ( 'NONE', #1004, 0.5000000000000022204 ) ;
#10476 = CARTESIAN_POINT ( 'NONE',  ( 47.63108361037843252, 56.43380494353993271, 10.49999999999999822 ) ) ;
#10477 = EDGE_LOOP ( 'NONE', ( #1274, #1600, #14204, #3269, #3239, #6943 ) ) ;
#10478 = FACE_OUTER_BOUND ( 'NONE', #6366, .T. ) ;
#10479 = EDGE_CURVE ( 'NONE', #345, #12576, #6804, .T. ) ;
#10480 = DIRECTION ( 'NONE',  ( 0.000000000000000000, 0.000000000000000000, 1.000000000000000000 ) ) ;
#10481 = AXIS2_PLACEMENT_3D ( 'NONE', #10357, #1249, #11433 ) ;
#10482 = ORIENTED_EDGE ( 'NONE', *, *, #6099, .F. ) ;
#10483 = CARTESIAN_POINT ( 'NONE',  ( 33.49014761921571193, 11.74264578624841171, -28.00000000000000000 ) ) ;
#10484 = CARTESIAN_POINT ( 'NONE',  ( 24.99999999999971934, 43.30127018922209459, 8.000000000000000000 ) ) ;
#10485 = CARTESIAN_POINT ( 'NONE',  ( 44.13108361037843252, 56.43380494353993271, 8.000000000000000000 ) ) ;
#10486 = DIRECTION ( 'NONE',  ( 1.000000000000000000, 0.000000000000000000, 0.000000000000000000 ) ) ;
#10487 = CARTESIAN_POINT ( 'NONE',  ( 0.000000000000000000, 0.000000000000000000, -5.000000000000000888 ) ) ;
#10488 = APPLICATION_PROTOCOL_DEFINITION ( 'draft international standard', 'automotive_design', 1998, #674 ) ;
#10489 = AXIS2_PLACEMENT_3D ( 'NONE', #10589, #5122, #9734 ) ;
#10490 = EDGE_CURVE ( 'NONE', #2772, #14249, #5601, .T. ) ;
#10491 = LINE ( 'NONE', #9635, #13885 ) ;
#10492 = ORIENTED_EDGE ( 'NONE', *, *, #133, .T. ) ;
#10493 = CARTESIAN_POINT ( 'NONE',  ( -10.55213320575001923, 106.4787665061024313, -18.97395805252363843 ) ) ;
#10494 = CARTESIAN_POINT ( 'NONE',  ( -68.49330278050074128, 68.09867107463051639, -10.50000000000000000 ) ) ;
#10495 = CIRCLE ( 'NONE', #6126, 2.041999999999999815 ) ;
#10496 = DIRECTION ( 'NONE',  ( 0.000000000000000000, 0.000000000000000000, 1.000000000000000000 ) ) ;
#10497 = CARTESIAN_POINT ( 'NONE',  ( 5.000000000000006217, 0.000000000000000000, -2.699999999999972644 ) ) ;
#10498 = AXIS2_PLACEMENT_3D ( 'NONE', #8146, #2147, #12629 ) ;
#10499 = ORIENTED_EDGE ( 'NONE', *, *, #1891, .T. ) ;
#10500 = CARTESIAN_POINT ( 'NONE',  ( 24.98583958711423492, -30.74264578624780597, -28.00000000000000000 ) ) ;
#10501 = ORIENTED_EDGE ( 'NONE', *, *, #5877, .T. ) ;
#10502 = CIRCLE ( 'NONE', #12451, 57.00000000000000000 ) ;
#10503 = CARTESIAN_POINT ( 'NONE',  ( 50.00000000000000000, 6.123233995736766085E-15, 8.000000000000000000 ) ) ;
#10504 = DIRECTION ( 'NONE',  ( -0.000000000000000000, -0.000000000000000000, 1.000000000000000000 ) ) ;
#10505 = AXIS2_PLACEMENT_3D ( 'NONE', #336, #10874, #14232 ) ;
#10506 = CARTESIAN_POINT ( 'NONE',  ( 12.50000000000000000, 40.62019202317980415, 16.00000000000000000 ) ) ;
#10507 = CARTESIAN_POINT ( 'NONE',  ( -6.917888187662729393, -52.54657765281195481, -10.50000000000000000 ) ) ;
#10508 = ORIENTED_EDGE ( 'NONE', *, *, #4552, .T. ) ;
#10509 = CIRCLE ( 'NONE', #2269, 2.649999999999985700 ) ;
#10510 = CARTESIAN_POINT ( 'NONE',  ( 25.00000000000000000, 81.24038404635960831, 26.00000000000000000 ) ) ;
#10511 = LINE ( 'NONE', #2461, #2539 ) ;
#10512 = CARTESIAN_POINT ( 'NONE',  ( 89.61631465359468507, -37.12029293941410657, -8.000000000000000000 ) ) ;
#10513 = ADVANCED_FACE ( 'NONE', ( #1364 ), #14189, .F. ) ;
#10514 = ORIENTED_EDGE ( 'NONE', *, *, #10346, .F. ) ;
#10515 = EDGE_CURVE ( 'NONE', #5248, #12429, #4843, .T. ) ;
#10516 = AXIS2_PLACEMENT_3D ( 'NONE', #5946, #10810, #5040 ) ;
#10517 = ORIENTED_EDGE ( 'NONE', *, *, #11827, .F. ) ;
#10518 = ORIENTED_EDGE ( 'NONE', *, *, #8969, .F. ) ;
#10519 = DIRECTION ( 'NONE',  ( -1.000000000000000000, 0.000000000000000000, 0.000000000000000000 ) ) ;
#10520 = CARTESIAN_POINT ( 'NONE',  ( -36.14014761921588104, 11.74264578624790190, -25.50000000000000355 ) ) ;
#10521 = CARTESIAN_POINT ( 'NONE',  ( 52.54657765281197612, -6.917888187662545540, -10.50000000000000000 ) ) ;
#10522 = VECTOR ( 'NONE', #13930, 1000.000000000000000 ) ;
#10523 = CARTESIAN_POINT ( 'NONE',  ( -13.35619814848797837, 51.53979475227131246, -13.00000000000000178 ) ) ;
#10524 = AXIS2_PLACEMENT_3D ( 'NONE', #12468, #1984, #11027 ) ;
#10525 = CIRCLE ( 'NONE', #3991, 59.50000000000000000 ) ;
#10526 = AXIS2_PLACEMENT_3D ( 'NONE', #477, #14011, #12860 ) ;
#10527 = CARTESIAN_POINT ( 'NONE',  ( -10.44268084954785714, 94.42456965614839248, 19.05230465901501091 ) ) ;
#10528 = EDGE_LOOP ( 'NONE', ( #9853, #12979, #8765, #7935, #8229 ) ) ;
#10529 = PRODUCT_RELATED_PRODUCT_CATEGORY ( 'part', '', ( #11072 ) ) ;
#10530 = CARTESIAN_POINT ( 'NONE',  ( 4.101954839143203024, 2.368264730583012234, -3.681130640444375324 ) ) ;
#10531 = PLANE ( 'NONE',  #9165 ) ;
#10532 = ADVANCED_FACE ( 'NONE', ( #5066 ), #3938, .F. ) ;
#10533 = ORIENTED_EDGE ( 'NONE', *, *, #4347, .F. ) ;
#10534 = CIRCLE ( 'NONE', #5460, 95.00000000000001421 ) ;
#10535 = EDGE_LOOP ( 'NONE', ( #8104, #1927, #14442, #864 ) ) ;
#10536 = CARTESIAN_POINT ( 'NONE',  ( -49.54657765281192638, 6.917888187662934563, -8.000000000000000000 ) ) ;
#10537 = AXIS2_PLACEMENT_3D ( 'NONE', #7201, #2425, #387 ) ;
#10538 = CIRCLE ( 'NONE', #13446, 3.000000000000002665 ) ;
#10539 = ORIENTED_EDGE ( 'NONE', *, *, #7123, .T. ) ;
#10540 = DIRECTION ( 'NONE',  ( 0.9557692240748186796, 0.2941176470588241498, 1.531423350357148967E-16 ) ) ;
#10541 = CARTESIAN_POINT ( 'NONE',  ( -11.10403672352021331, 74.17481381252333961, 18.51301757891051025 ) ) ;
#10542 = FACE_OUTER_BOUND ( 'NONE', #6315, .T. ) ;
#10543 = CARTESIAN_POINT ( 'NONE',  ( 100.0000000000000000, 1.224646799147353217E-14, 13.00000000000000178 ) ) ;
#10544 = CARTESIAN_POINT ( 'NONE',  ( -9.706343076449424956, 74.36968214894433515, -19.49591231693629112 ) ) ;
#10545 = LINE ( 'NONE', #12535, #4844 ) ;
#10546 = EDGE_LOOP ( 'NONE', ( #8148, #1659, #9237, #1219, #10052, #9291, #13475, #383 ) ) ;
#10547 = AXIS2_PLACEMENT_3D ( 'NONE', #12341, #2007, #13706 ) ;
#10548 = AXIS2_PLACEMENT_3D ( 'NONE', #12485, #946, #12333 ) ;
#10549 = DIRECTION ( 'NONE',  ( -0.000000000000000000, -0.000000000000000000, -1.000000000000000000 ) ) ;
#10550 = VECTOR ( 'NONE', #1672, 1000.000000000000000 ) ;
#10551 = ORIENTED_EDGE ( 'NONE', *, *, #14241, .F. ) ;
#10552 = CARTESIAN_POINT ( 'NONE',  ( 97.00000000000000000, -3.384287605079545030E-13, -10.50000000000000000 ) ) ;
#10553 = ADVANCED_FACE ( 'NONE', ( #7336 ), #1508, .F. ) ;
#10554 = EDGE_CURVE ( 'NONE', #3770, #4485, #3419, .T. ) ;
#10555 = CIRCLE ( 'NONE', #12509, 3.000000000000002665 ) ;
#10556 = LINE ( 'NONE', #2584, #3260 ) ;
#10557 = ADVANCED_FACE ( 'NONE', ( #7254 ), #7419, .T. ) ;
#10558 = ORIENTED_EDGE ( 'NONE', *, *, #8474, .T. ) ;
#10559 = CARTESIAN_POINT ( 'NONE',  ( -57.06275842387042729, 9.706953719246069312, 8.000000000000000000 ) ) ;
#10560 = AXIS2_PLACEMENT_3D ( 'NONE', #1603, #13144, #13222 ) ;
#10561 = EDGE_CURVE ( 'NONE', #11882, #5656, #13851, .T. ) ;
#10562 = CARTESIAN_POINT ( 'NONE',  ( -34.62083247296263266, -87.95718916809180143, -8.000000000000000000 ) ) ;
#10563 = CARTESIAN_POINT ( 'NONE',  ( 12.86891638962116247, -56.43380494354001087, -13.00000000000000178 ) ) ;
#10564 = CARTESIAN_POINT ( 'NONE',  ( 0.000000000000000000, 0.000000000000000000, 10.50000000000000000 ) ) ;
#10565 = CYLINDRICAL_SURFACE ( 'NONE', #14536, 59.50000000000000000 ) ;
#10566 = AXIS2_PLACEMENT_3D ( 'NONE', #10066, #14479, #4155 ) ;
#10567 = EDGE_CURVE ( 'NONE', #14620, #7243, #5115, .T. ) ;
#10568 = CARTESIAN_POINT ( 'NONE',  ( -18.52941176470586981, 60.21346111671361001, 16.00000000000000000 ) ) ;
#10569 = AXIS2_PLACEMENT_3D ( 'NONE', #367, #7027, #4927 ) ;
#10570 = VERTEX_POINT ( 'NONE', #2720 ) ;
#10571 = CARTESIAN_POINT ( 'NONE',  ( 0.3198814748697589860, 4.434118497892181487, -0.3507732604232494666 ) ) ;
#10572 = CARTESIAN_POINT ( 'NONE',  ( 8.072481656125567895, 94.65682832148054615, -19.97535367358596403 ) ) ;
#10573 = DIRECTION ( 'NONE',  ( 0.000000000000000000, 0.000000000000000000, 1.000000000000000000 ) ) ;
#10574 = CARTESIAN_POINT ( 'NONE',  ( 0.000000000000000000, 0.000000000000000000, -31.00000000000000000 ) ) ;
#10575 = EDGE_CURVE ( 'NONE', #7243, #2878, #2442, .T. ) ;
#10576 = VERTEX_POINT ( 'NONE', #8335 ) ;
#10577 = AXIS2_PLACEMENT_3D ( 'NONE', #2910, #1999, #563 ) ;
#10578 = FACE_OUTER_BOUND ( 'NONE', #13423, .T. ) ;
#10579 = ORIENTED_EDGE ( 'NONE', *, *, #3665, .F. ) ;
#10580 = DIRECTION ( 'NONE',  ( 1.000000000000000000, 0.000000000000000000, 0.000000000000000000 ) ) ;
#10581 = DIRECTION ( 'NONE',  ( -0.000000000000000000, -0.000000000000000000, 1.000000000000000000 ) ) ;
#10582 = CARTESIAN_POINT ( 'NONE',  ( 49.00442420935993226, -30.80502811811213704, 10.49999999999999822 ) ) ;
#10583 = CARTESIAN_POINT ( 'NONE',  ( 0.000000000000000000, 0.000000000000000000, -10.50000000000000000 ) ) ;
#10584 = ORIENTED_EDGE ( 'NONE', *, *, #2597, .T. ) ;
#10585 = CIRCLE ( 'NONE', #13754, 3.000000000000002665 ) ;
#10586 = AXIS2_PLACEMENT_3D ( 'NONE', #9968, #1780, #6692 ) ;
#10587 = CARTESIAN_POINT ( 'NONE',  ( 0.000000000000000000, 0.000000000000000000, 10.50000000000000000 ) ) ;
#10588 = CYLINDRICAL_SURFACE ( 'NONE', #8094, 3.000000000000002665 ) ;
#10589 = CARTESIAN_POINT ( 'NONE',  ( -6.917888187662729393, -52.54657765281195481, -13.00000000000000178 ) ) ;
#10590 = VERTEX_POINT ( 'NONE', #13049 ) ;
#10591 = EDGE_LOOP ( 'NONE', ( #9993, #7190, #14149, #11777 ) ) ;
#10592 = ORIENTED_EDGE ( 'NONE', *, *, #13309, .F. ) ;
#10593 = DIRECTION ( 'NONE',  ( 1.000000000000000000, 0.000000000000000000, 0.000000000000000000 ) ) ;
#10594 = CARTESIAN_POINT ( 'NONE',  ( 0.000000000000000000, 0.000000000000000000, -8.000000000000000000 ) ) ;
#10595 = CARTESIAN_POINT ( 'NONE',  ( 1.999999999999989564, -3.464101615137775703, -3.142992957459243453 ) ) ;
#10596 = EDGE_CURVE ( 'NONE', #13414, #5762, #2689, .T. ) ;
#10597 = DIRECTION ( 'NONE',  ( 0.000000000000000000, 0.000000000000000000, 1.000000000000000000 ) ) ;
#10598 = ORIENTED_EDGE ( 'NONE', *, *, #13578, .T. ) ;
#10599 = ORIENTED_EDGE ( 'NONE', *, *, #13458, .F. ) ;
#10600 = ORIENTED_EDGE ( 'NONE', *, *, #2278, .F. ) ;
#10601 = FACE_OUTER_BOUND ( 'NONE', #358, .T. ) ;
#10602 = CARTESIAN_POINT ( 'NONE',  ( 37.12029293941379393, 89.61631465359479876, 8.000000000000000000 ) ) ;
#10603 = CARTESIAN_POINT ( 'NONE',  ( 8.635061085254619684, 62.40781208424768778, 19.90323072647615632 ) ) ;
#10604 = VERTEX_POINT ( 'NONE', #11997 ) ;
#10605 = VERTEX_POINT ( 'NONE', #12975 ) ;
#10606 = DIRECTION ( 'NONE',  ( 1.000000000000000000, 0.000000000000000000, 0.000000000000000000 ) ) ;
#10607 = ORIENTED_EDGE ( 'NONE', *, *, #9727, .F. ) ;
#10608 = DIRECTION ( 'NONE',  ( 0.000000000000000000, 0.000000000000000000, 1.000000000000000000 ) ) ;
#10609 = CARTESIAN_POINT ( 'NONE',  ( -12.39897948556635754, 73.96800191783272282, 16.00000000000000000 ) ) ;
#10610 = ADVANCED_FACE ( 'NONE', ( #8630 ), #12961, .T. ) ;
#10611 = DIRECTION ( 'NONE',  ( 1.000000000000000000, 0.000000000000000000, 0.000000000000000000 ) ) ;
#10612 = CARTESIAN_POINT ( 'NONE',  ( 0.000000000000000000, 0.000000000000000000, -8.000000000000000000 ) ) ;
#10613 = EDGE_CURVE ( 'NONE', #13122, #914, #11016, .T. ) ;
#10614 = EDGE_CURVE ( 'NONE', #13996, #3137, #12008, .T. ) ;
#10615 = VERTEX_POINT ( 'NONE', #12066 ) ;
#10616 = CYLINDRICAL_SURFACE ( 'NONE', #842, 5.000000000000001776 ) ;
#10617 = CIRCLE ( 'NONE', #11113, 56.99999999999999289 ) ;
#10618 = CARTESIAN_POINT ( 'NONE',  ( -6.117650515114348764, -53.20607447915235610, -10.50000000000000000 ) ) ;
#10619 = ORIENTED_EDGE ( 'NONE', *, *, #4545, .F. ) ;
#10620 = CARTESIAN_POINT ( 'NONE',  ( -3.999999999999998224, -1.539600717839010979, -3.300726591567081591 ) ) ;
#10621 = EDGE_LOOP ( 'NONE', ( #3486, #4233, #8661, #10999, #13928 ) ) ;
#10622 = VERTEX_POINT ( 'NONE', #1656 ) ;
#10623 = SHAPE_REPRESENTATION ( 'brake caliper housing', ( #5108 ), #14072 ) ;
#10624 = DIRECTION ( 'NONE',  ( -1.000000000000000000, 0.000000000000000000, 0.000000000000000000 ) ) ;
#10625 = DIRECTION ( 'NONE',  ( 0.000000000000000000, 0.000000000000000000, 1.000000000000000000 ) ) ;
#10626 = CARTESIAN_POINT ( 'NONE',  ( -10.43254889841015220, 62.13061131512488089, 19.05984907584256760 ) ) ;
#10627 = DIRECTION ( 'NONE',  ( -1.000000000000000000, 0.000000000000000000, 0.000000000000000000 ) ) ;
#10628 = DIRECTION ( 'NONE',  ( -0.000000000000000000, -0.000000000000000000, -1.000000000000000000 ) ) ;
#10629 = CARTESIAN_POINT ( 'NONE',  ( -51.49712671369403694, -14.70911110638321873, -10.50000000000000000 ) ) ;
#10630 = CYLINDRICAL_SURFACE ( 'NONE', #222, 3.000000000000002665 ) ;
#10631 = ORIENTED_EDGE ( 'NONE', *, *, #12416, .T. ) ;
#10632 = FACE_BOUND ( 'NONE', #3638, .T. ) ;
#10633 = EDGE_LOOP ( 'NONE', ( #6716, #2463, #1850, #1443 ) ) ;
#10634 = ADVANCED_FACE ( 'NONE', ( #6260 ), #516, .F. ) ;
#10635 = CARTESIAN_POINT ( 'NONE',  ( -3.492805317593278058, 46.55633131742322917, -10.50000000000000000 ) ) ;
#10636 = CARTESIAN_POINT ( 'NONE',  ( -47.21331623427138879, -33.48561063518577896, -10.50000000000000000 ) ) ;
#10637 = EDGE_CURVE ( 'NONE', #6344, #4010, #14171, .T. ) ;
#10638 = CARTESIAN_POINT ( 'NONE',  ( 37.12029293941379393, 89.61631465359479876, -10.50000000000000000 ) ) ;
#10639 = DIRECTION ( 'NONE',  ( -0.000000000000000000, -0.000000000000000000, 1.000000000000000000 ) ) ;
#10640 = EDGE_LOOP ( 'NONE', ( #13831, #11462, #894, #8573, #11003 ) ) ;
#10641 = CYLINDRICAL_SURFACE ( 'NONE', #7545, 60.50000000000000000 ) ;
#10642 = ORIENTED_EDGE ( 'NONE', *, *, #8850, .F. ) ;
#10643 = CARTESIAN_POINT ( 'NONE',  ( -14.00000000000000000, 0.000000000000000000, 14.49999999999999822 ) ) ;
#10644 = DIRECTION ( 'NONE',  ( 1.000000000000000000, 0.000000000000000000, -0.000000000000000000 ) ) ;
#10645 = AXIS2_PLACEMENT_3D ( 'NONE', #10018, #5310, #3050 ) ;
#10646 = CARTESIAN_POINT ( 'NONE',  ( 89.61631465359468507, -37.12029293941410657, -13.00000000000000178 ) ) ;
#10647 = FACE_OUTER_BOUND ( 'NONE', #8443, .T. ) ;
#10648 = EDGE_CURVE ( 'NONE', #1542, #10333, #3038, .T. ) ;
#10649 = ORIENTED_EDGE ( 'NONE', *, *, #12893, .F. ) ;
#10650 = ADVANCED_FACE ( 'NONE', ( #13420 ), #592, .F. ) ;
#10651 = CARTESIAN_POINT ( 'NONE',  ( 6.917888187663118416, 52.54657765281190507, 10.49999999999999822 ) ) ;
#10652 =( GEOMETRIC_REPRESENTATION_CONTEXT ( 3 ) GLOBAL_UNCERTAINTY_ASSIGNED_CONTEXT ( ( #12108 ) ) GLOBAL_UNIT_ASSIGNED_CONTEXT ( ( #12583, #2257, #1133 ) ) REPRESENTATION_CONTEXT ( 'NONE', 'WORKASPACE' ) );
#10653 = DIRECTION ( 'NONE',  ( 1.000000000000000000, 0.000000000000000000, 0.000000000000000000 ) ) ;
#10654 = AXIS2_PLACEMENT_3D ( 'NONE', #12987, #2578, #7194 ) ;
#10655 = DIRECTION ( 'NONE',  ( -1.000000000000000000, 0.000000000000000000, 0.000000000000000000 ) ) ;
#10656 = VECTOR ( 'NONE', #7039, 1000.000000000000000 ) ;
#10657 = AXIS2_PLACEMENT_3D ( 'NONE', #10409, #13841, #4575 ) ;
#10658 = ORIENTED_EDGE ( 'NONE', *, *, #9173, .T. ) ;
#10659 = EDGE_CURVE ( 'NONE', #10704, #13133, #14487, .T. ) ;
#10660 = ORIENTED_EDGE ( 'NONE', *, *, #6328, .T. ) ;
#10661 = CARTESIAN_POINT ( 'NONE',  ( 8.801203450618841018, 106.6379082728991534, 19.83890680725671274 ) ) ;
#10662 = CARTESIAN_POINT ( 'NONE',  ( -0.6507732100473468950, 4.243078065514775510, -0.2236248678334808448 ) ) ;
#10663 = VECTOR ( 'NONE', #9857, 1000.000000000000000 ) ;
#10664 = CARTESIAN_POINT ( 'NONE',  ( -37.71449950290985953, 86.67575032682117353, -13.00000000000000178 ) ) ;
#10665 = CARTESIAN_POINT ( 'NONE',  ( 0.000000000000000000, 0.000000000000000000, -8.000000000000000000 ) ) ;
#10666 = FILL_AREA_STYLE ('',( #1416 ) ) ;
#10667 = LINE ( 'NONE', #1568, #624 ) ;
#10668 = AXIS2_PLACEMENT_3D ( 'NONE', #14828, #2068, #12472 ) ;
#10669 = VERTEX_POINT ( 'NONE', #2866 ) ;
#10670 = VERTEX_POINT ( 'NONE', #11301 ) ;
#10671 = CIRCLE ( 'NONE', #9220, 4.000000000000000000 ) ;
#10672 = ORIENTED_EDGE ( 'NONE', *, *, #6202, .T. ) ;
#10673 = ORIENTED_EDGE ( 'NONE', *, *, #252, .F. ) ;
#10674 = B_SPLINE_CURVE_WITH_KNOTS ( 'NONE', 3,
 ( #4850, #6754, #9470, #12981, #8264, #9327, #14116, #7191, #6689, #3572, #11844, #10544, #5492, #8189, #12552, #2414, #3723, #12479 ),
 .UNSPECIFIED., .F., .F.,
 ( 4, 2, 2, 2, 2, 2, 2, 2, 4 ),
 ( 0.001002962753164631828, 0.001858089309406474668, 0.002713215865648317508, 0.003568342421890159915, 0.004423468978132002322, 0.005278595534373845162, 0.006133722090615688002, 0.006988848646857530843, 0.007843975203099373683 ),
 .UNSPECIFIED. ) ;
#10675 = DIRECTION ( 'NONE',  ( 0.000000000000000000, 0.000000000000000000, 1.000000000000000000 ) ) ;
#10676 = DIRECTION ( 'NONE',  ( 1.000000000000000000, 0.000000000000000000, -0.000000000000000000 ) ) ;
#10677 = CARTESIAN_POINT ( 'NONE',  ( 20.00000000000000000, 64.99230723708768664, -31.00000000000000000 ) ) ;
#10678 = VERTEX_POINT ( 'NONE', #1949 ) ;
#10679 = CIRCLE ( 'NONE', #10205, 53.55662432702593634 ) ;
#10680 = ORIENTED_EDGE ( 'NONE', *, *, #6776, .T. ) ;
#10681 = CARTESIAN_POINT ( 'NONE',  ( 0.000000000000000000, 0.000000000000000000, -13.00000000000000178 ) ) ;
#10682 = CIRCLE ( 'NONE', #7270, 3.000000000000002665 ) ;
#10683 = ORIENTED_EDGE ( 'NONE', *, *, #13266, .T. ) ;
#10684 = AXIS2_PLACEMENT_3D ( 'NONE', #1978, #2057, #10104 ) ;
#10685 = AXIS2_PLACEMENT_3D ( 'NONE', #2847, #6394, #1560 ) ;
#10686 = DIRECTION ( 'NONE',  ( 0.000000000000000000, 0.000000000000000000, 1.000000000000000000 ) ) ;
#10687 = CARTESIAN_POINT ( 'NONE',  ( -11.55014193876141171, 53.26842454702440222, 8.000000000000000000 ) ) ;
#10688 = CARTESIAN_POINT ( 'NONE',  ( -33.48561063518626923, 47.21331623427104063, -13.00000000000000178 ) ) ;
#10689 = AXIS2_PLACEMENT_3D ( 'NONE', #12685, #13906, #11480 ) ;
#10690 = EDGE_LOOP ( 'NONE', ( #12969, #9920, #7681, #9414, #5124, #13717 ) ) ;
#10692 = CIRCLE ( 'NONE', #6562, 0.5000000000000038858 ) ;
#10691 = DIRECTION ( 'NONE',  ( 0.000000000000000000, 0.000000000000000000, -1.000000000000000000 ) ) ;
#10693 = DIRECTION ( 'NONE',  ( 0.000000000000000000, 0.000000000000000000, 1.000000000000000000 ) ) ;
#10694 = ORIENTED_EDGE ( 'NONE', *, *, #5681, .T. ) ;
#10695 = CIRCLE ( 'NONE', #6806, 5.000000000000001776 ) ;
#10696 = CARTESIAN_POINT ( 'NONE',  ( -12.86891638962156215, 56.43380494353993271, -13.00000000000000178 ) ) ;
#10697 = AXIS2_PLACEMENT_3D ( 'NONE', #4891, #11588, #9420 ) ;
#10698 = VERTEX_POINT ( 'NONE', #3022 ) ;
#10699 = EDGE_CURVE ( 'NONE', #1593, #508, #6392, .T. ) ;
#10700 = EDGE_LOOP ( 'NONE', ( #8935, #5972, #2896, #1420, #10025 ) ) ;
#10701 =( LENGTH_UNIT ( ) NAMED_UNIT ( * ) SI_UNIT ( .MILLI., .METRE. ) );
#10702 = EDGE_CURVE ( 'NONE', #13295, #5812, #6646, .T. ) ;
#10703 = ADVANCED_FACE ( 'NONE', ( #4090 ), #5451, .T. ) ;
#10704 = VERTEX_POINT ( 'NONE', #13275 ) ;
#10705 = CIRCLE ( 'NONE', #9490, 5.000000000000000888 ) ;
#10706 = DIRECTION ( 'NONE',  ( 1.000000000000000000, 0.000000000000000000, 0.000000000000000000 ) ) ;
#10707 = CARTESIAN_POINT ( 'NONE',  ( 31.77701906416544020, 102.1706497334997721, -12.77113345645743792 ) ) ;
#10708 = CIRCLE ( 'NONE', #1985, 59.50000000000000000 ) ;
#10709 = DIRECTION ( 'NONE',  ( 0.000000000000000000, 0.000000000000000000, -1.000000000000000000 ) ) ;
#10710 = DIRECTION ( 'NONE',  ( 0.000000000000000000, 0.000000000000000000, 1.000000000000000000 ) ) ;
#10711 = DIRECTION ( 'NONE',  ( 0.000000000000000000, 0.000000000000000000, -1.000000000000000000 ) ) ;
#10712 = EDGE_CURVE ( 'NONE', #1597, #11013, #11723, .T. ) ;
#10713 = DIRECTION ( 'NONE',  ( 0.000000000000000000, 0.000000000000000000, 1.000000000000000000 ) ) ;
#10714 = ORIENTED_EDGE ( 'NONE', *, *, #5096, .T. ) ;
#10715 = SURFACE_STYLE_FILL_AREA ( #1610 ) ;
#10716 = VECTOR ( 'NONE', #2473, 999.9999999999998863 ) ;
#10717 = ORIENTED_EDGE ( 'NONE', *, *, #2963, .T. ) ;
#10718 = ADVANCED_FACE ( 'NONE', ( #5293 ), #1732, .F. ) ;
#10719 = LINE ( 'NONE', #7060, #6442 ) ;
#10720 = PLANE ( 'NONE',  #8074 ) ;
#10721 = VECTOR ( 'NONE', #4208, 1000.000000000000000 ) ;
#10722 = DIRECTION ( 'NONE',  ( 0.000000000000000000, 0.000000000000000000, -1.000000000000000000 ) ) ;
#10723 = EDGE_CURVE ( 'NONE', #571, #12166, #8780, .T. ) ;
#10724 = CARTESIAN_POINT ( 'NONE',  ( -68.68541276968778675, 69.08004447556137961, -13.00000000000000178 ) ) ;
#10725 = ORIENTED_EDGE ( 'NONE', *, *, #9588, .F. ) ;
#10726 = DIRECTION ( 'NONE',  ( 0.000000000000000000, 0.000000000000000000, 1.000000000000000000 ) ) ;
#10727 = ORIENTED_EDGE ( 'NONE', *, *, #5474, .T. ) ;
#10728 = CARTESIAN_POINT ( 'NONE',  ( 0.000000000000000000, 0.000000000000000000, -45.50000000000000000 ) ) ;
#10729 = CARTESIAN_POINT ( 'NONE',  ( 0.000000000000000000, 0.000000000000000000, -8.000000000000000000 ) ) ;
#10730 = CARTESIAN_POINT ( 'NONE',  ( 3.999999999999996447, 0.000000000000000000, 0.000000000000000000 ) ) ;
#10731 = AXIS2_PLACEMENT_3D ( 'NONE', #13684, #4795, #6836 ) ;
#10732 = CARTESIAN_POINT ( 'NONE',  ( 0.000000000000000000, 0.000000000000000000, -45.50000000000000000 ) ) ;
#10733 = ORIENTED_EDGE ( 'NONE', *, *, #12412, .F. ) ;
#10734 = B_SPLINE_CURVE_WITH_KNOTS ( 'NONE', 3,
 ( #14998, #1327, #2378, #6928, #3455, #1177, #5943, #6993 ),
 .UNSPECIFIED., .F., .F.,
 ( 4, 2, 2, 4 ),
 ( 0.005725059856848643478, 0.006314084072593628347, 0.006903108288338612349, 0.008081156719828581220 ),
 .UNSPECIFIED. ) ;
#10735 = DIRECTION ( 'NONE',  ( 1.000000000000000000, 0.000000000000000000, 0.000000000000000000 ) ) ;
#10736 = PLANE ( 'NONE',  #5212 ) ;
#10737 = VECTOR ( 'NONE', #14695, 1000.000000000000000 ) ;
#10738 = DIRECTION ( 'NONE',  ( -1.000000000000000000, 0.000000000000000000, 0.000000000000000000 ) ) ;
#10739 = ORIENTED_EDGE ( 'NONE', *, *, #14758, .F. ) ;
#10740 = CARTESIAN_POINT ( 'NONE',  ( -2.836893136758492862, -3.208949435745870105, -3.505054077164886372 ) ) ;
#10741 = EDGE_CURVE ( 'NONE', #9388, #5971, #14642, .T. ) ;
#10742 = AXIS2_PLACEMENT_3D ( 'NONE', #2011, #13479, #7626 ) ;
#10743 = VERTEX_POINT ( 'NONE', #11222 ) ;
#10744 = ADVANCED_FACE ( 'NONE', ( #14784 ), #824, .T. ) ;
#10745 = PLANE ( 'NONE',  #13455 ) ;
#10746 = EDGE_LOOP ( 'NONE', ( #3750, #6581, #3466, #9295 ) ) ;
#10747 = EDGE_CURVE ( 'NONE', #14193, #12545, #1095, .T. ) ;
#10748 = AXIS2_PLACEMENT_3D ( 'NONE', #7178, #2791, #13269 ) ;
#10749 = DIRECTION ( 'NONE',  ( 0.000000000000000000, 0.000000000000000000, 1.000000000000000000 ) ) ;
#10750 = DIRECTION ( 'NONE',  ( 0.000000000000000000, 0.000000000000000000, -1.000000000000000000 ) ) ;
#10751 = DIRECTION ( 'NONE',  ( 0.000000000000000000, 0.000000000000000000, 1.000000000000000000 ) ) ;
#10752 = VERTEX_POINT ( 'NONE', #1806 ) ;
#10753 = EDGE_CURVE ( 'NONE', #8417, #1677, #10538, .T. ) ;
#10754 = DIRECTION ( 'NONE',  ( 0.000000000000000000, 0.000000000000000000, 1.000000000000000000 ) ) ;
#10755 = CARTESIAN_POINT ( 'NONE',  ( -49.00442420935969778, 30.80502811811250297, -8.000000000000000000 ) ) ;
#10756 = AXIS2_PLACEMENT_3D ( 'NONE', #13628, #5356, #9984 ) ;
#10757 = CARTESIAN_POINT ( 'NONE',  ( 19.99999999999999645, 64.99230723708767243, 26.00000000000000000 ) ) ;
#10758 = ORIENTED_EDGE ( 'NONE', *, *, #11602, .T. ) ;
#10759 = ORIENTED_EDGE ( 'NONE', *, *, #13266, .F. ) ;
#10760 = DIRECTION ( 'NONE',  ( 1.000000000000000000, 0.000000000000000000, 0.000000000000000000 ) ) ;
#10761 = VERTEX_POINT ( 'NONE', #10992 ) ;
#10762 = EDGE_CURVE ( 'NONE', #2772, #5947, #5226, .T. ) ;
#10763 = VECTOR ( 'NONE', #12030, 1000.000000000000000 ) ;
#10764 = CIRCLE ( 'NONE', #6886, 20.00000000000000000 ) ;
#10765 = CARTESIAN_POINT ( 'NONE',  ( 57.06275842387049835, -9.706953719245678514, -8.000000000000000000 ) ) ;
#10766 = AXIS2_PLACEMENT_3D ( 'NONE', #10039, #870, #9805 ) ;
#10767 = CARTESIAN_POINT ( 'NONE',  ( -0.2790467552932217599, 96.58511096861892042, -13.00000000000000178 ) ) ;
#10768 = DIRECTION ( 'NONE',  ( 1.000000000000000000, 0.000000000000000000, 0.000000000000000000 ) ) ;
#10769 = ORIENTED_EDGE ( 'NONE', *, *, #722, .F. ) ;
#10770 = CARTESIAN_POINT ( 'NONE',  ( 36.14014761921570340, 11.74264578624841171, -28.00000000000000000 ) ) ;
#10771 = DIRECTION ( 'NONE',  ( 0.000000000000000000, 0.000000000000000000, 1.000000000000000000 ) ) ;
#10772 = ORIENTED_EDGE ( 'NONE', *, *, #12158, .F. ) ;
#10773 = CARTESIAN_POINT ( 'NONE',  ( 2.449293598294700991E-16, -97.00000000000000000, -13.00000000000000178 ) ) ;
#10774 = AXIS2_PLACEMENT_3D ( 'NONE', #11709, #4867, #9481 ) ;
#10775 = EDGE_LOOP ( 'NONE', ( #4097, #14422, #5647, #58, #8071, #2795 ) ) ;
#10776 = AXIS2_PLACEMENT_3D ( 'NONE', #7562, #14564, #6489 ) ;
#10777 = ORIENTED_EDGE ( 'NONE', *, *, #7268, .F. ) ;
#10778 = CARTESIAN_POINT ( 'NONE',  ( 0.000000000000000000, 0.000000000000000000, -45.50000000000000000 ) ) ;
#10779 = DIRECTION ( 'NONE',  ( 0.000000000000000000, 0.000000000000000000, 1.000000000000000000 ) ) ;
#10780 = DIRECTION ( 'NONE',  ( -1.000000000000000000, 0.000000000000000000, 0.000000000000000000 ) ) ;
#10781 = CIRCLE ( 'NONE', #3034, 0.5000000000000004441 ) ;
#10782 = AXIS2_PLACEMENT_3D ( 'NONE', #583, #9834, #11294 ) ;
#10783 = DIRECTION ( 'NONE',  ( 1.000000000000000000, 0.000000000000000000, 0.000000000000000000 ) ) ;
#10784 = CARTESIAN_POINT ( 'NONE',  ( 0.000000000000000000, 0.000000000000000000, -10.50000000000000000 ) ) ;
#10785 = CARTESIAN_POINT ( 'NONE',  ( 0.000000000000000000, 0.000000000000000000, -10.50000000000000000 ) ) ;
#10786 = ADVANCED_FACE ( 'NONE', ( #7793 ), #7617, .T. ) ;
#10787 = EDGE_CURVE ( 'NONE', #13104, #14416, #2529, .T. ) ;
#10788 = AXIS2_PLACEMENT_3D ( 'NONE', #12918, #7052, #3437 ) ;
#10789 = DIRECTION ( 'NONE',  ( 0.000000000000000000, 0.000000000000000000, 1.000000000000000000 ) ) ;
#10790 = ORIENTED_EDGE ( 'NONE', *, *, #6420, .F. ) ;
#10791 = EDGE_CURVE ( 'NONE', #14250, #10988, #12490, .T. ) ;
#10792 = DIRECTION ( 'NONE',  ( 1.000000000000000000, 0.000000000000000000, 0.000000000000000000 ) ) ;
#10793 = ADVANCED_FACE ( 'NONE', ( #5667 ), #11372, .T. ) ;
#10794 = ORIENTED_EDGE ( 'NONE', *, *, #9144, .T. ) ;
#10795 = DIRECTION ( 'NONE',  ( 0.000000000000000000, 1.000000000000000000, -1.287488025362403787E-15 ) ) ;
#10796 = CARTESIAN_POINT ( 'NONE',  ( 45.89934640057532533, -26.49999999999987566, -13.00000000000000178 ) ) ;
#10797 = CARTESIAN_POINT ( 'NONE',  ( 12.50000000000000000, 59.24038404635959409, 20.00000000000000000 ) ) ;
#10798 = AXIS2_PLACEMENT_3D ( 'NONE', #11771, #8113, #14964 ) ;
#10799 = CARTESIAN_POINT ( 'NONE',  ( -33.48561063518626923, 47.21331623427104063, -8.000000000000000000 ) ) ;
#10800 = ORIENTED_EDGE ( 'NONE', *, *, #3078, .F. ) ;
#10801 = CARTESIAN_POINT ( 'NONE',  ( 4.198928548860770604, -0.8158838809860120556, -3.526471437616916837 ) ) ;
#10802 = ORIENTED_EDGE ( 'NONE', *, *, #8286, .F. ) ;
#10803 = ORIENTED_EDGE ( 'NONE', *, *, #2296, .F. ) ;
#10804 = EDGE_CURVE ( 'NONE', #7348, #10294, #4246, .T. ) ;
#10805 = DIRECTION ( 'NONE',  ( -0.000000000000000000, -0.000000000000000000, -1.000000000000000000 ) ) ;
#10806 = CARTESIAN_POINT ( 'NONE',  ( 89.61631465359468507, -37.12029293941410657, 8.000000000000000000 ) ) ;
#10807 = AXIS2_PLACEMENT_3D ( 'NONE', #10894, #498, #9745 ) ;
#10808 = AXIS2_PLACEMENT_3D ( 'NONE', #11238, #6662, #10316 ) ;
#10809 = CARTESIAN_POINT ( 'NONE',  ( 2.500000000000002220, -1.178949249685222522, -2.042000000000002036 ) ) ;
#10810 = DIRECTION ( 'NONE',  ( 0.000000000000000000, 0.000000000000000000, -1.000000000000000000 ) ) ;
#10811 = EDGE_CURVE ( 'NONE', #2518, #4822, #852, .T. ) ;
#10812 = EDGE_CURVE ( 'NONE', #14416, #13104, #9551, .T. ) ;
#10813 = CARTESIAN_POINT ( 'NONE',  ( -11.46115996437298357, 94.30629603967057051, 18.06445797889986338 ) ) ;
#10814 = ORIENTED_EDGE ( 'NONE', *, *, #11333, .T. ) ;
#10815 = CARTESIAN_POINT ( 'NONE',  ( 0.000000000000000000, 0.000000000000000000, -10.50000000000000000 ) ) ;
#10816 = DIRECTION ( 'NONE',  ( 1.000000000000000000, 0.000000000000000000, 0.000000000000000000 ) ) ;
#10817 = LINE ( 'NONE', #418, #8542 ) ;
#10818 = AXIS2_PLACEMENT_3D ( 'NONE', #2691, #2613, #13093 ) ;
#10819 = VERTEX_POINT ( 'NONE', #4467 ) ;
#10820 = CARTESIAN_POINT ( 'NONE',  ( -87.95718916809170196, 34.62083247296289557, 8.000000000000000000 ) ) ;
#10821 = ORIENTED_EDGE ( 'NONE', *, *, #9620, .F. ) ;
#10822 = FACE_OUTER_BOUND ( 'NONE', #12048, .T. ) ;
#10823 = DIRECTION ( 'NONE',  ( -0.000000000000000000, -0.000000000000000000, 1.000000000000000000 ) ) ;
#10824 = FACE_OUTER_BOUND ( 'NONE', #13316, .T. ) ;
#10825 =( NAMED_UNIT ( * ) SI_UNIT ( $, .STERADIAN. ) SOLID_ANGLE_UNIT ( ) );
#10826 = CARTESIAN_POINT ( 'NONE',  ( 68.01302780753354682, -65.64523757230297463, -13.00000000000000178 ) ) ;
#10827 = CIRCLE ( 'NONE', #12289, 2.500000000000000444 ) ;
#10828 = ORIENTED_EDGE ( 'NONE', *, *, #9676, .F. ) ;
#10829 = CARTESIAN_POINT ( 'NONE',  ( 97.50000000000000000, -3.384287605079545030E-13, -13.00000000000000178 ) ) ;
#10830 = DIRECTION ( 'NONE',  ( -1.000000000000000000, 0.000000000000000000, -0.000000000000000000 ) ) ;
#10831 = EDGE_CURVE ( 'NONE', #9394, #6432, #5914, .T. ) ;
#10832 = CARTESIAN_POINT ( 'NONE',  ( 0.2500000000000002220, 0.000000000000000000, 4.000000000000000000 ) ) ;
#10833 = ORIENTED_EDGE ( 'NONE', *, *, #6268, .T. ) ;
#10834 = EDGE_CURVE ( 'NONE', #5876, #11296, #2253, .T. ) ;
#10835 = ORIENTED_EDGE ( 'NONE', *, *, #13081, .F. ) ;
#10836 = CARTESIAN_POINT ( 'NONE',  ( -37.12029293941250074, 89.61631465359532456, -8.000000000000000000 ) ) ;
#10837 = ORIENTED_EDGE ( 'NONE', *, *, #12268, .T. ) ;
#10838 = DIRECTION ( 'NONE',  ( -1.000000000000000000, 0.000000000000000000, 0.000000000000000000 ) ) ;
#10839 = EDGE_CURVE ( 'NONE', #12197, #14062, #6888, .T. ) ;
#10840 = CARTESIAN_POINT ( 'NONE',  ( -4.154094228333817362, -2.398367420967598029, -3.721909803043260023 ) ) ;
#10841 = PLANE ( 'NONE',  #1952 ) ;
#10842 = ORIENTED_EDGE ( 'NONE', *, *, #13396, .F. ) ;
#10843 = CARTESIAN_POINT ( 'NONE',  ( 0.000000000000000000, -1.178949249685208533, 2.042000000000002036 ) ) ;
#10844 = DIRECTION ( 'NONE',  ( -1.000000000000000000, 0.000000000000000000, 0.000000000000000000 ) ) ;
#10845 = EDGE_LOOP ( 'NONE', ( #8915, #13348 ) ) ;
#10846 = CARTESIAN_POINT ( 'NONE',  ( 26.00011991137315803, 45.91029614918951296, 10.49999999999999822 ) ) ;
#10847 = EDGE_CURVE ( 'NONE', #5358, #13983, #467, .T. ) ;
#10848 = ADVANCED_FACE ( 'NONE', ( #7865 ), #4483, .T. ) ;
#10849 = ORIENTED_EDGE ( 'NONE', *, *, #9856, .F. ) ;
#10850 = VERTEX_POINT ( 'NONE', #2328 ) ;
#10851 = CARTESIAN_POINT ( 'NONE',  ( -70.71067811865387398, 70.71067811865562192, 8.000000000000000000 ) ) ;
#10852 = DIRECTION ( 'NONE',  ( -1.000000000000000000, 0.000000000000000000, 0.000000000000000000 ) ) ;
#10853 = ADVANCED_FACE ( 'NONE', ( #10443 ), #46, .T. ) ;
#10854 = CLOSED_SHELL ( 'NONE', ( #4693, #12334, #10343, #9633, #11037, #14339, #10368, #24, #6984, #6941, #5107, #13437, #7005, #10703, #11093, #1353, #14900, #9254, #2672, #8115, #11382, #12068, #2777, #13868, #12978, #9311, #8051 ) ) ;
#10855 = CARTESIAN_POINT ( 'NONE',  ( -31.74999999999995737, 0.000000000000000000, 4.249999999999972466 ) ) ;
#10856 = CYLINDRICAL_SURFACE ( 'NONE', #1479, 0.5000000000000004441 ) ;
#10857 = CARTESIAN_POINT ( 'NONE',  ( 1.655952806101429031, -3.662737355149044749, -8.872387778173047248E-15 ) ) ;
#10858 = CARTESIAN_POINT ( 'NONE',  ( 41.59008834022645829, 32.46576781417968505, 10.49999999999999822 ) ) ;
#10859 = ORIENTED_EDGE ( 'NONE', *, *, #7489, .F. ) ;
#10860 = CARTESIAN_POINT ( 'NONE',  ( -6.917888187662729393, -52.54657765281195481, -8.000000000000000000 ) ) ;
#10861 = ORIENTED_EDGE ( 'NONE', *, *, #11049, .F. ) ;
#10862 = DIRECTION ( 'NONE',  ( -1.000000000000000000, 0.000000000000000000, 0.000000000000000000 ) ) ;
#10863 = CARTESIAN_POINT ( 'NONE',  ( -91.27544013909712817, 39.61975340586647576, 8.000000000000000000 ) ) ;
#10864 = VERTEX_POINT ( 'NONE', #1266 ) ;
#10865 = DIRECTION ( 'NONE',  ( -1.000000000000000000, -1.065907399692639811E-13, 0.000000000000000000 ) ) ;
#10866 = DIRECTION ( 'NONE',  ( -1.000000000000000000, 0.000000000000000000, 0.000000000000000000 ) ) ;
#10867 = ORIENTED_EDGE ( 'NONE', *, *, #8788, .F. ) ;
#10868 = DIRECTION ( 'NONE',  ( 0.000000000000000000, 0.000000000000000000, 1.000000000000000000 ) ) ;
#10869 = ORIENTED_EDGE ( 'NONE', *, *, #9617, .T. ) ;
#10870 = ORIENTED_EDGE ( 'NONE', *, *, #5708, .T. ) ;
#10871 = FACE_OUTER_BOUND ( 'NONE', #2024, .T. ) ;
#10872 = CARTESIAN_POINT ( 'NONE',  ( -33.29654390035820910, 41.94820822869202459, -10.50000000000000000 ) ) ;
#10873 = CARTESIAN_POINT ( 'NONE',  ( -7.500000000000000888, 106.7368258849775202, 20.00000000000000355 ) ) ;
#10874 = DIRECTION ( 'NONE',  ( 0.000000000000000000, 0.000000000000000000, 1.000000000000000000 ) ) ;
#10875 = DIRECTION ( 'NONE',  ( 1.000000000000000000, 1.826024711554534012E-15, 0.000000000000000000 ) ) ;
#10876 = ORIENTED_EDGE ( 'NONE', *, *, #10648, .F. ) ;
#10877 = DIRECTION ( 'NONE',  ( 1.000000000000000000, 0.000000000000000000, 0.000000000000000000 ) ) ;
#10878 = CYLINDRICAL_SURFACE ( 'NONE', #6405, 56.99999999999998579 ) ;
#10879 = DIRECTION ( 'NONE',  ( 0.000000000000000000, 0.000000000000000000, -1.000000000000000000 ) ) ;
#10880 = ADVANCED_FACE ( 'NONE', ( #12804 ), #2391, .F. ) ;
#10881 = UNCERTAINTY_MEASURE_WITH_UNIT (LENGTH_MEASURE( 1.000000000000000082E-05 ), #11982, 'distance_accuracy_value', 'NONE');
#10882 = ADVANCED_FACE ( 'NONE', ( #14165 ), #12254, .T. ) ;
#10883 = ORIENTED_EDGE ( 'NONE', *, *, #11687, .T. ) ;
#10884 = EDGE_CURVE ( 'NONE', #2594, #8099, #8829, .T. ) ;
#10885 = EDGE_CURVE ( 'NONE', #1920, #6713, #3516, .T. ) ;
#10886 = DIRECTION ( 'NONE',  ( 0.000000000000000000, -1.224646799147353454E-16, 1.000000000000000000 ) ) ;
#10887 = EDGE_LOOP ( 'NONE', ( #6840, #8086, #14052, #7790 ) ) ;
#10888 = ADVANCED_FACE ( 'NONE', ( #14521 ), #5261, .F. ) ;
#10889 = CARTESIAN_POINT ( 'NONE',  ( 0.000000000000000000, 0.000000000000000000, -25.50000000000000355 ) ) ;
#10890 = LINE ( 'NONE', #8682, #9730 ) ;
#10891 = CARTESIAN_POINT ( 'NONE',  ( 12.86891638962116247, -56.43380494354001087, -10.50000000000000000 ) ) ;
#10892 = FACE_BOUND ( 'NONE', #11278, .T. ) ;
#10893 = DIRECTION ( 'NONE',  ( -1.000000000000000000, 0.000000000000000000, 6.123233995736766036E-17 ) ) ;
#10894 = CARTESIAN_POINT ( 'NONE',  ( -13.71740939043329277, 51.19406879332069593, -8.000000000000000000 ) ) ;
#10895 = EDGE_CURVE ( 'NONE', #8551, #1906, #9785, .T. ) ;
#10896 = PRESENTATION_LAYER_ASSIGNMENT (  '', '', ( #2405 ) ) ;
#10897 = B_SPLINE_CURVE_WITH_KNOTS ( 'NONE', 3,
 ( #6227, #405, #6162, #470 ),
 .UNSPECIFIED., .F., .F.,
 ( 4, 4 ),
 ( 0.000000000000000000, 0.001005167940839974024 ),
 .UNSPECIFIED. ) ;
#10898 = EDGE_LOOP ( 'NONE', ( #10199, #10923, #12916 ) ) ;
#10899 = CARTESIAN_POINT ( 'NONE',  ( 36.70371619500516402, 89.33979373934434420, -10.50000000000000000 ) ) ;
#10900 = AXIS2_PLACEMENT_3D ( 'NONE', #4417, #1751, #14504 ) ;
#10901 = FACE_OUTER_BOUND ( 'NONE', #630, .T. ) ;
#10902 = DIRECTION ( 'NONE',  ( 0.5000000000000009992, -6.123233995736778362E-17, 0.8660254037844380415 ) ) ;
#10903 = ORIENTED_EDGE ( 'NONE', *, *, #9613, .T. ) ;
#10904 = ORIENTED_EDGE ( 'NONE', *, *, #1378, .F. ) ;
#10905 = CARTESIAN_POINT ( 'NONE',  ( 0.000000000000000000, 0.000000000000000000, -16.00000000000000000 ) ) ;
#10906 = ORIENTED_EDGE ( 'NONE', *, *, #14202, .T. ) ;
#10907 = CIRCLE ( 'NONE', #11648, 3.000000000000004441 ) ;
#10908 = AXIS2_PLACEMENT_3D ( 'NONE', #3606, #14075, #9212 ) ;
#10909 = DIRECTION ( 'NONE',  ( 0.000000000000000000, 0.000000000000000000, 1.000000000000000000 ) ) ;
#10910 = AXIS2_PLACEMENT_3D ( 'NONE', #14997, #8218, #14073 ) ;
#10911 = ADVANCED_FACE ( 'NONE', ( #8395 ), #2622, .T. ) ;
#10912 = AXIS2_PLACEMENT_3D ( 'NONE', #9342, #5849, #4729 ) ;
#10913 = CARTESIAN_POINT ( 'NONE',  ( 3.436319922986348807, -2.634841920958731709, -3.531542292954501505 ) ) ;
#10914 = ORIENTED_EDGE ( 'NONE', *, *, #4652, .F. ) ;
#10915 = DIRECTION ( 'NONE',  ( 0.000000000000000000, 0.000000000000000000, 1.000000000000000000 ) ) ;
#10916 = DIRECTION ( 'NONE',  ( 0.000000000000000000, 0.000000000000000000, 1.000000000000000000 ) ) ;
#10917 = VERTEX_POINT ( 'NONE', #11894 ) ;
#10918 = DIRECTION ( 'NONE',  ( 1.000000000000000000, -4.440892098500626162E-15, 0.000000000000000000 ) ) ;
#10919 = CIRCLE ( 'NONE', #1713, 56.99999999999999289 ) ;
#10920 = ORIENTED_EDGE ( 'NONE', *, *, #12563, .T. ) ;
#10921 = CIRCLE ( 'NONE', #8489, 60.50000000000000000 ) ;
#10922 = MECHANICAL_DESIGN_GEOMETRIC_PRESENTATION_REPRESENTATION (  '', ( #4862 ), #4141 ) ;
#10923 = ORIENTED_EDGE ( 'NONE', *, *, #5373, .T. ) ;
#10924 = CYLINDRICAL_SURFACE ( 'NONE', #1357, 59.50000000000000711 ) ;
#10925 = CARTESIAN_POINT ( 'NONE',  ( 32.65070903206050446, 101.8685403450051155, -14.31792419690431650 ) ) ;
#10926 = CIRCLE ( 'NONE', #3417, 3.000000000000002665 ) ;
#10927 = EDGE_CURVE ( 'NONE', #11092, #10391, #9564, .T. ) ;
#10928 = AXIS2_PLACEMENT_3D ( 'NONE', #207, #8478, #6123 ) ;
#10929 = EDGE_CURVE ( 'NONE', #2375, #7147, #94, .T. ) ;
#10930 = DIRECTION ( 'NONE',  ( -0.000000000000000000, -0.000000000000000000, 1.000000000000000000 ) ) ;
#10931 = DIRECTION ( 'NONE',  ( 1.000000000000000000, 0.000000000000000000, 0.000000000000000000 ) ) ;
#10932 = DIRECTION ( 'NONE',  ( 0.000000000000000000, -1.000000000000000000, 0.000000000000000000 ) ) ;
#10933 = AXIS2_PLACEMENT_3D ( 'NONE', #8089, #5883, #10445 ) ;
#10934 = CARTESIAN_POINT ( 'NONE',  ( 69.16568774265594755, -71.53347797788796925, -13.00000000000000178 ) ) ;
#10935 = AXIS2_PLACEMENT_3D ( 'NONE', #10082, #9921, #14571 ) ;
#10936 = ORIENTED_EDGE ( 'NONE', *, *, #6862, .T. ) ;
#10937 = LINE ( 'NONE', #14437, #11671 ) ;
#10938 = ORIENTED_EDGE ( 'NONE', *, *, #9164, .T. ) ;
#10939 = ADVANCED_FACE ( 'NONE', ( #1488 ), #11034, .T. ) ;
#10940 = DIRECTION ( 'NONE',  ( 1.000000000000000000, 0.000000000000000000, 0.000000000000000000 ) ) ;
#10941 = DIRECTION ( 'NONE',  ( -0.000000000000000000, -0.000000000000000000, -1.000000000000000000 ) ) ;
#10942 = AXIS2_PLACEMENT_3D ( 'NONE', #12520, #9806, #10875 ) ;
#10943 = VERTEX_POINT ( 'NONE', #7168 ) ;
#10944 = DIRECTION ( 'NONE',  ( -0.000000000000000000, -0.000000000000000000, -1.000000000000000000 ) ) ;
#10945 = EDGE_LOOP ( 'NONE', ( #3785, #1025, #2978, #6269 ) ) ;
#10946 = CARTESIAN_POINT ( 'NONE',  ( -90.10640870805754332, -37.02125851216322872, -13.00000000000000178 ) ) ;
#10947 = VECTOR ( 'NONE', #12493, 1000.000000000000000 ) ;
#10948 = ORIENTED_EDGE ( 'NONE', *, *, #11876, .T. ) ;
#10949 = DIRECTION ( 'NONE',  ( 0.000000000000000000, 0.000000000000000000, 1.000000000000000000 ) ) ;
#10950 = VERTEX_POINT ( 'NONE', #10952 ) ;
#10951 = EDGE_CURVE ( 'NONE', #3168, #2447, #5184, .T. ) ;
#10952 = CARTESIAN_POINT ( 'NONE',  ( -7.500000000000000888, 106.7368258849775202, -20.00000000000000000 ) ) ;
#10953 = CARTESIAN_POINT ( 'NONE',  ( -36.70371619500578220, -89.33979373934407420, -13.00000000000000178 ) ) ;
#10954 = PLANE ( 'NONE',  #4923 ) ;
#10955 = AXIS2_PLACEMENT_3D ( 'NONE', #10040, #12328, #4356 ) ;
#10956 = DIRECTION ( 'NONE',  ( -0.000000000000000000, -0.000000000000000000, 1.000000000000000000 ) ) ;
#10957 = FACE_OUTER_BOUND ( 'NONE', #11254, .T. ) ;
#10958 = DIRECTION ( 'NONE',  ( -1.000000000000000000, 0.000000000000000000, 0.000000000000000000 ) ) ;
#10959 = B_SPLINE_CURVE_WITH_KNOTS ( 'NONE', 3,
 ( #3415, #10394, #6962, #10662, #6814, #64 ),
 .UNSPECIFIED., .F., .F.,
 ( 4, 2, 4 ),
 ( 0.002365888236227972966, 0.003551327329835076308, 0.004736766423442179651 ),
 .UNSPECIFIED. ) ;
#10960 = ORIENTED_EDGE ( 'NONE', *, *, #9207, .T. ) ;
#10961 = CIRCLE ( 'NONE', #3447, 0.5000000000000022204 ) ;
#10962 = CARTESIAN_POINT ( 'NONE',  ( 37.62029293941316155, -89.61631465359504034, -10.50000000000000000 ) ) ;
#10963 = CYLINDRICAL_SURFACE ( 'NONE', #10046, 22.00000000000001421 ) ;
#10964 = LINE ( 'NONE', #9816, #12200 ) ;
#10965 = ORIENTED_EDGE ( 'NONE', *, *, #8446, .F. ) ;
#10966 = VECTOR ( 'NONE', #2768, 1000.000000000000000 ) ;
#10967 = ORIENTED_EDGE ( 'NONE', *, *, #6657, .T. ) ;
#10968 = DIRECTION ( 'NONE',  ( -0.000000000000000000, -0.000000000000000000, -1.000000000000000000 ) ) ;
#10969 = ORIENTED_EDGE ( 'NONE', *, *, #4957, .T. ) ;
#10970 = AXIS2_PLACEMENT_3D ( 'NONE', #3977, #1691, #3905 ) ;
#10971 = CARTESIAN_POINT ( 'NONE',  ( -7.500000000000000888, 59.24038404635959409, -15.00000000000000000 ) ) ;
#10972 = DIRECTION ( 'NONE',  ( -0.000000000000000000, -0.000000000000000000, -1.000000000000000000 ) ) ;
#10973 = CARTESIAN_POINT ( 'NONE',  ( 0.000000000000000000, 0.000000000000000000, -20.00000000000000000 ) ) ;
#10974 = DIRECTION ( 'NONE',  ( 0.000000000000000000, 0.000000000000000000, 1.000000000000000000 ) ) ;
#10975 = DIRECTION ( 'NONE',  ( 1.000000000000000000, 0.000000000000000000, 0.000000000000000000 ) ) ;
#10976 = CARTESIAN_POINT ( 'NONE',  ( 31.47058823529413374, 102.2673069760056563, -10.99999999999999645 ) ) ;
#10977 = ORIENTED_EDGE ( 'NONE', *, *, #14991, .T. ) ;
#10978 = AXIS2_PLACEMENT_3D ( 'NONE', #4248, #11145, #5526 ) ;
#10979 = EDGE_LOOP ( 'NONE', ( #8476, #7654, #13386, #3051, #9402, #6563, #2953, #8271, #9837 ) ) ;
#10980 = CIRCLE ( 'NONE', #3469, 10.00000000000000178 ) ;
#10981 = EDGE_CURVE ( 'NONE', #9738, #2014, #7389, .T. ) ;
#10982 = DIRECTION ( 'NONE',  ( 0.000000000000000000, 0.000000000000000000, 1.000000000000000000 ) ) ;
#10984 = ADVANCED_FACE ( 'NONE', ( #7088 ), #2220, .F. ) ;
#10983 = DIRECTION ( 'NONE',  ( 1.000000000000000000, 0.000000000000000000, 0.000000000000000000 ) ) ;
#10985 = DIRECTION ( 'NONE',  ( 0.000000000000000000, -1.000000000000000000, 0.000000000000000000 ) ) ;
#10986 = VERTEX_POINT ( 'NONE', #12619 ) ;
#10987 = AXIS2_PLACEMENT_3D ( 'NONE', #809, #13404, #11207 ) ;
#10988 = VERTEX_POINT ( 'NONE', #2067 ) ;
#10989 = DIRECTION ( 'NONE',  ( -1.000000000000000000, 0.000000000000000000, 0.000000000000000000 ) ) ;
#10990 = ORIENTED_EDGE ( 'NONE', *, *, #2721, .F. ) ;
#10991 = AXIS2_PLACEMENT_3D ( 'NONE', #2099, #11135, #11065 ) ;
#10992 = CARTESIAN_POINT ( 'NONE',  ( -100.0000000000000000, 1.047191897158270473E-12, 8.000000000000000000 ) ) ;
#10993 = CARTESIAN_POINT ( 'NONE',  ( 4.236525694536555697, -2.416953475386484751, -3.751298745799840795 ) ) ;
#10994 = EDGE_CURVE ( 'NONE', #6159, #7414, #12017, .T. ) ;
#10995 = DIRECTION ( 'NONE',  ( 1.000000000000000000, 0.000000000000000000, 0.000000000000000000 ) ) ;
#10996 = AXIS2_PLACEMENT_3D ( 'NONE', #10507, #4670, #2092 ) ;
#10997 = CARTESIAN_POINT ( 'NONE',  ( -37.12029293941250074, 89.61631465359532456, 8.000000000000000000 ) ) ;
#10998 = CARTESIAN_POINT ( 'NONE',  ( -33.32140965599871407, 101.6077678005751324, 14.98557208302583632 ) ) ;
#10999 = ORIENTED_EDGE ( 'NONE', *, *, #1034, .F. ) ;
#11000 = ADVANCED_FACE ( 'NONE', ( #11338 ), #11257, .F. ) ;
#11001 = CARTESIAN_POINT ( 'NONE',  ( 2.171643655288381325, -3.365003104552330537, -9.498909814825474384E-15 ) ) ;
#11002 = AXIS2_PLACEMENT_3D ( 'NONE', #12350, #3012, #13636 ) ;
#11003 = ORIENTED_EDGE ( 'NONE', *, *, #2217, .T. ) ;
#11004 = VERTEX_POINT ( 'NONE', #11185 ) ;
#11005 = CARTESIAN_POINT ( 'NONE',  ( -32.93386454278234510, 95.47976343162785895, 15.73819668677757910 ) ) ;
#11006 = CIRCLE ( 'NONE', #4472, 44.89637028918153305 ) ;
#11007 = AXIS2_PLACEMENT_3D ( 'NONE', #10583, #182, #4815 ) ;
#11008 = DIRECTION ( 'NONE',  ( 0.000000000000000000, 0.000000000000000000, -1.000000000000000000 ) ) ;
#11009 = DIRECTION ( 'NONE',  ( 0.000000000000000000, 0.000000000000000000, 1.000000000000000000 ) ) ;
#11010 = DIRECTION ( 'NONE',  ( 0.000000000000000000, 0.000000000000000000, -1.000000000000000000 ) ) ;
#11011 = DIRECTION ( 'NONE',  ( 0.000000000000000000, 0.000000000000000000, 1.000000000000000000 ) ) ;
#11012 = CARTESIAN_POINT ( 'NONE',  ( -36.70371619500578220, -89.33979373934407420, 10.49999999999999822 ) ) ;
#11013 = VERTEX_POINT ( 'NONE', #3066 ) ;
#11014 = AXIS2_PLACEMENT_3D ( 'NONE', #11490, #5623, #1087 ) ;
#11015 = FACE_OUTER_BOUND ( 'NONE', #6498, .T. ) ;
#11016 = CIRCLE ( 'NONE', #4731, 56.99999999999999289 ) ;
#11017 = FACE_OUTER_BOUND ( 'NONE', #11459, .T. ) ;
#11018 = DIRECTION ( 'NONE',  ( 1.000000000000000000, 0.000000000000000000, 0.000000000000000000 ) ) ;
#11019 = EDGE_CURVE ( 'NONE', #2144, #6138, #6902, .T. ) ;
#11020 = DIRECTION ( 'NONE',  ( 1.000000000000000000, 0.000000000000000000, 0.000000000000000000 ) ) ;
#11021 = EDGE_CURVE ( 'NONE', #7084, #8152, #5554, .T. ) ;
#11022 = EDGE_CURVE ( 'NONE', #9994, #15024, #9799, .T. ) ;
#11023 = EDGE_LOOP ( 'NONE', ( #6346, #8054, #7491 ) ) ;
#11024 = CARTESIAN_POINT ( 'NONE',  ( 32.93386454278233799, 95.47976343162785895, -15.73819668677757555 ) ) ;
#11025 = ORIENTED_EDGE ( 'NONE', *, *, #5593, .T. ) ;
#11026 = AXIS2_PLACEMENT_3D ( 'NONE', #10681, #291, #8410 ) ;
#11027 = DIRECTION ( 'NONE',  ( 1.000000000000000000, 0.000000000000000000, 0.000000000000000000 ) ) ;
#11028 = ORIENTED_EDGE ( 'NONE', *, *, #11417, .F. ) ;
#11029 = AXIS2_PLACEMENT_3D ( 'NONE', #12202, #1574, #12058 ) ;
#11030 = AXIS2_PLACEMENT_3D ( 'NONE', #7770, #12413, #8761 ) ;
#11031 = CARTESIAN_POINT ( 'NONE',  ( 4.197393957002300446, 7.760817478283647932E-14, -3.503767560748928922 ) ) ;
#11032 = VECTOR ( 'NONE', #6140, 1000.000000000000000 ) ;
#11033 = ORIENTED_EDGE ( 'NONE', *, *, #4781, .F. ) ;
#11034 = PLANE ( 'NONE',  #14919 ) ;
#11035 = DIRECTION ( 'NONE',  ( 0.000000000000000000, 0.000000000000000000, 1.000000000000000000 ) ) ;
#11036 = DIRECTION ( 'NONE',  ( 0.000000000000000000, 0.000000000000000000, 1.000000000000000000 ) ) ;
#11037 = ADVANCED_FACE ( 'NONE', ( #4285 ), #8893, .T. ) ;
#11038 = CARTESIAN_POINT ( 'NONE',  ( 9.706953719245472456, 57.06275842387054098, 10.49999999999999822 ) ) ;
#11039 = CARTESIAN_POINT ( 'NONE',  ( 13.35619814848834075, -51.53979475227123430, -10.50000000000000000 ) ) ;
#11040 = VERTEX_POINT ( 'NONE', #13766 ) ;
#11041 = CARTESIAN_POINT ( 'NONE',  ( 47.21331623427115431, 33.48561063518610581, -13.00000000000000178 ) ) ;
#11042 = AXIS2_PLACEMENT_3D ( 'NONE', #8212, #12849, #2443 ) ;
#11043 = EDGE_LOOP ( 'NONE', ( #3334, #10842, #14163, #12952 ) ) ;
#11044 = AXIS2_PLACEMENT_3D ( 'NONE', #4369, #3306, #954 ) ;
#11045 = CARTESIAN_POINT ( 'NONE',  ( 7.500000000000000888, 74.62405778299650194, -20.00000000000000000 ) ) ;
#11046 = DIRECTION ( 'NONE',  ( 1.000000000000000000, 0.000000000000000000, 0.000000000000000000 ) ) ;
#11047 = AXIS2_PLACEMENT_3D ( 'NONE', #14808, #11321, #7581 ) ;
#11048 = EDGE_CURVE ( 'NONE', #2937, #14795, #5464, .T. ) ;
#11049 = EDGE_CURVE ( 'NONE', #8993, #3488, #8602, .T. ) ;
#11050 = DIRECTION ( 'NONE',  ( -0.000000000000000000, -0.000000000000000000, 1.000000000000000000 ) ) ;
#11051 = ORIENTED_EDGE ( 'NONE', *, *, #12718, .T. ) ;
#11052 = AXIS2_PLACEMENT_3D ( 'NONE', #3622, #14947, #12882 ) ;
#11053 = DIRECTION ( 'NONE',  ( 0.000000000000000000, 0.000000000000000000, -1.000000000000000000 ) ) ;
#11054 = ORIENTED_EDGE ( 'NONE', *, *, #12338, .T. ) ;
#11055 = DIRECTION ( 'NONE',  ( 0.000000000000000000, 0.000000000000000000, 1.000000000000000000 ) ) ;
#11056 = CARTESIAN_POINT ( 'NONE',  ( 0.000000000000000000, 0.000000000000000000, -10.50000000000000000 ) ) ;
#11057 = CARTESIAN_POINT ( 'NONE',  ( 12.28299834225913045, 61.79111542428975667, -16.56818924177462904 ) ) ;
#11058 = DIRECTION ( 'NONE',  ( 1.000000000000000000, 0.000000000000000000, 0.000000000000000000 ) ) ;
#11059 = DIRECTION ( 'NONE',  ( 0.000000000000000000, 0.000000000000000000, 1.000000000000000000 ) ) ;
#11060 = ORIENTED_EDGE ( 'NONE', *, *, #2649, .T. ) ;
#11061 = VERTEX_POINT ( 'NONE', #7973 ) ;
#11062 = CIRCLE ( 'NONE', #13251, 3.000000000000002665 ) ;
#11063 = CARTESIAN_POINT ( 'NONE',  ( 0.000000000000000000, 4.618802153517009401, -3.433295621305381573 ) ) ;
#11064 = CARTESIAN_POINT ( 'NONE',  ( 86.67575032682076142, 37.71449950291080455, 8.000000000000000000 ) ) ;
#11065 = DIRECTION ( 'NONE',  ( 1.000000000000000000, 0.000000000000000000, -0.000000000000000000 ) ) ;
#11066 = ORIENTED_EDGE ( 'NONE', *, *, #4552, .F. ) ;
#11067 = ORIENTED_EDGE ( 'NONE', *, *, #8762, .T. ) ;
#11068 = EDGE_LOOP ( 'NONE', ( #5752, #8223, #9143, #2156, #8312 ) ) ;
#11069 = EDGE_CURVE ( 'NONE', #4578, #10105, #4084, .T. ) ;
#11070 = AXIS2_PLACEMENT_3D ( 'NONE', #169, #3745, #1458 ) ;
#11071 = DIRECTION ( 'NONE',  ( 0.000000000000000000, 0.000000000000000000, 1.000000000000000000 ) ) ;
#11072 = PRODUCT ( 'brake pad', 'brake pad', '', ( #2093 ) ) ;
#11073 = CARTESIAN_POINT ( 'NONE',  ( 47.21331623427115431, 33.48561063518610581, -10.50000000000000000 ) ) ;
#11074 = LINE ( 'NONE', #5296, #13643 ) ;
#11075 = ORIENTED_EDGE ( 'NONE', *, *, #3879, .T. ) ;
#11076 = DIRECTION ( 'NONE',  ( -0.000000000000000000, -0.000000000000000000, 1.000000000000000000 ) ) ;
#11077 = DIRECTION ( 'NONE',  ( -1.000000000000000000, 0.000000000000000000, 0.000000000000000000 ) ) ;
#11078 = VERTEX_POINT ( 'NONE', #14905 ) ;
#11079 = DIRECTION ( 'NONE',  ( -1.000000000000000000, 0.000000000000000000, 0.000000000000000000 ) ) ;
#11080 = AXIS2_PLACEMENT_3D ( 'NONE', #4960, #3822, #4884 ) ;
#11081 = VERTEX_POINT ( 'NONE', #4429 ) ;
#11082 = VERTEX_POINT ( 'NONE', #9039 ) ;
#11083 = CARTESIAN_POINT ( 'NONE',  ( -30.68753049492183749, 96.22530292649338435, 14.05553407057507620 ) ) ;
#11084 = ADVANCED_FACE ( 'NONE', ( #13682 ), #3284, .F. ) ;
#11085 = EDGE_CURVE ( 'NONE', #8383, #14537, #2542, .T. ) ;
#11086 = ADVANCED_FACE ( 'NONE', ( #3354 ), #8816, .T. ) ;
#11087 = DIRECTION ( 'NONE',  ( -1.000000000000000000, 0.000000000000000000, 0.000000000000000000 ) ) ;
#11088 = PRODUCT_DEFINITION_CONTEXT ( 'detailed design', #5236, 'design' ) ;
#11089 = FACE_OUTER_BOUND ( 'NONE', #6554, .T. ) ;
#11090 = LINE ( 'NONE', #6507, #13099 ) ;
#11091 = FACE_OUTER_BOUND ( 'NONE', #2243, .T. ) ;
#11092 = VERTEX_POINT ( 'NONE', #7 ) ;
#11093 = ADVANCED_FACE ( 'NONE', ( #10407 ), #3736, .T. ) ;
#11094 = EDGE_CURVE ( 'NONE', #9519, #2565, #3528, .T. ) ;
#11095 = CARTESIAN_POINT ( 'NONE',  ( 22.33583958711425055, -30.74264578624780597, -28.00000000000000000 ) ) ;
#11096 = ORIENTED_EDGE ( 'NONE', *, *, #8873, .F. ) ;
#11097 = CARTESIAN_POINT ( 'NONE',  ( -45.91029614918924295, 26.00011991137363765, -13.00000000000000178 ) ) ;
#11098 = FACE_OUTER_BOUND ( 'NONE', #2472, .T. ) ;
#11099 = ORIENTED_EDGE ( 'NONE', *, *, #11826, .F. ) ;
#11100 = PRESENTATION_STYLE_ASSIGNMENT (( #6449 ) ) ;
#11101 = CARTESIAN_POINT ( 'NONE',  ( -94.51066581171356518, -1.674280531758327140, -13.00000000000000178 ) ) ;
#11102 = AXIS2_PLACEMENT_3D ( 'NONE', #7877, #6724, #2266 ) ;
#11103 = EDGE_LOOP ( 'NONE', ( #9440, #5459, #6744, #10539, #4177 ) ) ;
#11104 = DIRECTION ( 'NONE',  ( 0.000000000000000000, 0.000000000000000000, 1.000000000000000000 ) ) ;
#11105 = VERTEX_POINT ( 'NONE', #10484 ) ;
#11106 = CARTESIAN_POINT ( 'NONE',  ( 12.18091848848563608, 106.3044177073317087, 16.76518324937863014 ) ) ;
#11107 = CARTESIAN_POINT ( 'NONE',  ( 27.01438936481372721, 47.21331623427104063, 10.49999999999999822 ) ) ;
#11108 = CARTESIAN_POINT ( 'NONE',  ( 0.000000000000000000, 0.000000000000000000, 13.00000000000000178 ) ) ;
#11109 = CARTESIAN_POINT ( 'NONE',  ( -26.49999999999971578, -45.89934640057541060, -13.00000000000000178 ) ) ;
#11110 = ADVANCED_FACE ( 'NONE', ( #12998 ), #14978, .T. ) ;
#11111 = DIRECTION ( 'NONE',  ( 0.000000000000000000, 0.000000000000000000, 1.000000000000000000 ) ) ;
#11112 = DIRECTION ( 'NONE',  ( 1.000000000000000000, 0.000000000000000000, 0.000000000000000000 ) ) ;
#11113 = AXIS2_PLACEMENT_3D ( 'NONE', #10755, #13192, #4081 ) ;
#11114 = ADVANCED_FACE ( 'NONE', ( #5991 ), #8057, .F. ) ;
#11115 = ORIENTED_EDGE ( 'NONE', *, *, #2040, .F. ) ;
#11116 = CARTESIAN_POINT ( 'NONE',  ( 10.21287289150292743, 74.30275811153845211, -19.23918552186209041 ) ) ;
#11117 = CARTESIAN_POINT ( 'NONE',  ( -22.05882352941176450, 71.68269180561142662, -23.50000000000000000 ) ) ;
#11118 = B_SPLINE_CURVE_WITH_KNOTS ( 'NONE', 3,
 ( #762, #4184, #684, #12223, #450, #11005, #9929, #8794, #1820, #613, #2810, #10011, #11083, #6273, #13432, #3040, #7660, #5079, #12303, #5391 ),
 .UNSPECIFIED., .F., .F.,
 ( 4, 2, 2, 2, 2, 2, 2, 2, 2, 4 ),
 ( 0.000000000000000000, 0.0009765940263104732309, 0.001464891039465707027, 0.001953188052620940824, 0.002929782078931390202, 0.003906376105241839147, 0.004882970131552281587, 0.005859564157862724894, 0.006836158184173168201, 0.007812752210483610640 ),
 .UNSPECIFIED. ) ;
#11119 = CARTESIAN_POINT ( 'NONE',  ( 3.999999999999998224, 0.8378280264232922381, -3.220590601395640906 ) ) ;
#11120 = B_SPLINE_CURVE_WITH_KNOTS ( 'NONE', 3,
 ( #3068, #7828, #5415, #13603, #5263 ),
 .UNSPECIFIED., .F., .F.,
 ( 4, 1, 4 ),
 ( 0.000000000000000000, 0.002309401076758505356, 0.004618802153517009845 ),
 .UNSPECIFIED. ) ;
#11121 = ORIENTED_EDGE ( 'NONE', *, *, #7408, .F. ) ;
#11122 = CARTESIAN_POINT ( 'NONE',  ( 25.00000000000000000, 81.24038404635960831, -16.00000000000000000 ) ) ;
#11123 = EDGE_LOOP ( 'NONE', ( #3124, #14088, #12443, #10124, #9674 ) ) ;
#11124 = CYLINDRICAL_SURFACE ( 'NONE', #4493, 59.50000000000000000 ) ;
#11125 = EDGE_CURVE ( 'NONE', #7436, #2855, #12415, .T. ) ;
#11126 = DIRECTION ( 'NONE',  ( 0.000000000000000000, 0.000000000000000000, 1.000000000000000000 ) ) ;
#11127 = ADVANCED_FACE ( 'NONE', ( #12837 ), #4871, .F. ) ;
#11128 = DIRECTION ( 'NONE',  ( -1.000000000000000000, 0.000000000000000000, 0.000000000000000000 ) ) ;
#11129 = DIRECTION ( 'NONE',  ( 0.000000000000000000, 0.000000000000000000, 1.000000000000000000 ) ) ;
#11130 = EDGE_LOOP ( 'NONE', ( #2523, #10439, #7116, #10777 ) ) ;
#11131 = VERTEX_POINT ( 'NONE', #3586 ) ;
#11132 = ORIENTED_EDGE ( 'NONE', *, *, #11520, .T. ) ;
#11133 = CARTESIAN_POINT ( 'NONE',  ( -51.19406879332065330, -13.71740939043347041, 8.000000000000000000 ) ) ;
#11134 = CARTESIAN_POINT ( 'NONE',  ( -47.00000000000000000, 81.24038404635962252, -26.00000000000000000 ) ) ;
#11135 = DIRECTION ( 'NONE',  ( 0.000000000000000000, 0.000000000000000000, 1.000000000000000000 ) ) ;
#11136 = ORIENTED_EDGE ( 'NONE', *, *, #3332, .T. ) ;
#11137 = ADVANCED_FACE ( 'NONE', ( #3655 ), #13838, .T. ) ;
#11138 = AXIS2_PLACEMENT_3D ( 'NONE', #2050, #9023, #13584 ) ;
#11139 = ORIENTED_EDGE ( 'NONE', *, *, #11689, .T. ) ;
#11140 = ORIENTED_EDGE ( 'NONE', *, *, #14471, .T. ) ;
#11141 = CARTESIAN_POINT ( 'NONE',  ( 23.51438936481372366, 47.21331623427104063, -13.00000000000000178 ) ) ;
#11142 = COLOUR_RGB ( '', 0.08235294, 0.09019608, 0.10196078) ;
#11143 = EDGE_CURVE ( 'NONE', #406, #11311, #2428, .T. ) ;
#11144 = DIRECTION ( 'NONE',  ( 0.000000000000000000, 0.000000000000000000, 1.000000000000000000 ) ) ;
#11145 = DIRECTION ( 'NONE',  ( -0.000000000000000000, -0.000000000000000000, 1.000000000000000000 ) ) ;
#11146 = VECTOR ( 'NONE', #12457, 1000.000000000000000 ) ;
#11147 = CARTESIAN_POINT ( 'NONE',  ( -15.88467684210512942, 49.11971303961693280, 8.000000000000000000 ) ) ;
#11148 = DIRECTION ( 'NONE',  ( 1.000000000000000000, 0.000000000000000000, 0.000000000000000000 ) ) ;
#11149 = ORIENTED_EDGE ( 'NONE', *, *, #7637, .F. ) ;
#11150 = CARTESIAN_POINT ( 'NONE',  ( -38.26834323650970049, -92.38795325112837986, -8.000000000000000000 ) ) ;
#11151 = ORIENTED_EDGE ( 'NONE', *, *, #11937, .T. ) ;
#11152 = ORIENTED_EDGE ( 'NONE', *, *, #918, .F. ) ;
#11153 = AXIS2_PLACEMENT_3D ( 'NONE', #4328, #8790, #11079 ) ;
#11155 = ORIENTED_EDGE ( 'NONE', *, *, #14901, .F. ) ;
#11154 =( REPRESENTATION_RELATIONSHIP ('NONE','NONE', #12187, #8006 ) REPRESENTATION_RELATIONSHIP_WITH_TRANSFORMATION ( #14774 )SHAPE_REPRESENTATION_RELATIONSHIP( ) );
#11156 = DIRECTION ( 'NONE',  ( 0.000000000000000000, 0.000000000000000000, 1.000000000000000000 ) ) ;
#11157 = AXIS2_PLACEMENT_3D ( 'NONE', #3085, #10056, #14704 ) ;
#11158 = CIRCLE ( 'NONE', #7015, 20.00000000000000000 ) ;
#11159 = AXIS2_PLACEMENT_3D ( 'NONE', #6279, #10932, #7280 ) ;
#11160 = CARTESIAN_POINT ( 'NONE',  ( 0.000000000000000000, 0.000000000000000000, -8.000000000000000000 ) ) ;
#11161 = CARTESIAN_POINT ( 'NONE',  ( -48.19406879332065330, -13.71740939043347041, -13.00000000000000178 ) ) ;
#11162 = DIRECTION ( 'NONE',  ( 1.000000000000000000, 0.000000000000000000, 0.000000000000000000 ) ) ;
#11163 = CIRCLE ( 'NONE', #11895, 3.000000000000002665 ) ;
#11164 = CARTESIAN_POINT ( 'NONE',  ( 0.000000000000000000, 0.000000000000000000, 20.00000000000000355 ) ) ;
#11165 = ORIENTED_EDGE ( 'NONE', *, *, #1747, .F. ) ;
#11166 = EDGE_CURVE ( 'NONE', #9753, #9297, #14434, .T. ) ;
#11167 = AXIS2_PLACEMENT_3D ( 'NONE', #7867, #13730, #4034 ) ;
#11168 = DIRECTION ( 'NONE',  ( 0.000000000000000000, 0.000000000000000000, -1.000000000000000000 ) ) ;
#11169 = ADVANCED_FACE ( 'NONE', ( #9483 ), #1225, .T. ) ;
#11170 = CARTESIAN_POINT ( 'NONE',  ( 42.04772703543530099, 32.26435573746242369, 10.49999999999999822 ) ) ;
#11171 = DIRECTION ( 'NONE',  ( 0.000000000000000000, 0.000000000000000000, 1.000000000000000000 ) ) ;
#11172 = EDGE_CURVE ( 'NONE', #362, #6726, #11789, .T. ) ;
#11173 = ORIENTED_EDGE ( 'NONE', *, *, #11085, .T. ) ;
#11174 = AXIS2_PLACEMENT_3D ( 'NONE', #10165, #6739, #5476 ) ;
#11175 = EDGE_LOOP ( 'NONE', ( #5735, #3305, #9137, #12684 ) ) ;
#11176 = AXIS2_PLACEMENT_3D ( 'NONE', #7030, #990, #13094 ) ;
#11177 = FACE_OUTER_BOUND ( 'NONE', #13592, .T. ) ;
#11178 = VERTEX_POINT ( 'NONE', #2361 ) ;
#11179 = LINE ( 'NONE', #10029, #13105 ) ;
#11180 = EDGE_CURVE ( 'NONE', #4586, #2764, #9268, .T. ) ;
#11181 = AXIS2_PLACEMENT_3D ( 'NONE', #11821, #3619, #9444 ) ;
#11182 = ORIENTED_EDGE ( 'NONE', *, *, #10328, .F. ) ;
#11183 = AXIS2_PLACEMENT_3D ( 'NONE', #14195, #2804, #1512 ) ;
#11184 = ORIENTED_EDGE ( 'NONE', *, *, #206, .T. ) ;
#11185 = CARTESIAN_POINT ( 'NONE',  ( -24.99999999999972644, -43.30127018922209459, -8.000000000000000000 ) ) ;
#11186 = DIRECTION ( 'NONE',  ( -0.000000000000000000, -0.000000000000000000, 1.000000000000000000 ) ) ;
#11187 = CARTESIAN_POINT ( 'NONE',  ( -36.14014761921588104, 11.74264578624790190, 14.49999999999999822 ) ) ;
#11188 = DIRECTION ( 'NONE',  ( 1.000000000000000000, 0.000000000000000000, 0.000000000000000000 ) ) ;
#11189 = CARTESIAN_POINT ( 'NONE',  ( 0.000000000000000000, 0.000000000000000000, -13.00000000000000178 ) ) ;
#11190 = CARTESIAN_POINT ( 'NONE',  ( -42.00000000000000000, 81.24038404635962252, -26.00000000000000000 ) ) ;
#11191 = ORIENTED_EDGE ( 'NONE', *, *, #1376, .T. ) ;
#11192 = EDGE_CURVE ( 'NONE', #7885, #5519, #14130, .T. ) ;
#11193 = DIRECTION ( 'NONE',  ( -1.000000000000000000, 1.776356839400250465E-15, 0.000000000000000000 ) ) ;
#11194 = AXIS2_PLACEMENT_3D ( 'NONE', #9880, #476, #5039 ) ;
#11195 = FACE_OUTER_BOUND ( 'NONE', #3624, .T. ) ;
#11196 = AXIS2_PLACEMENT_3D ( 'NONE', #3753, #11653, #10421 ) ;
#11197 = CARTESIAN_POINT ( 'NONE',  ( 4.203935335434015208, 1.640780671294171045, -3.598452447879191052 ) ) ;
#11198 = PRODUCT_DEFINITION_SHAPE ( 'NONE', 'NONE',  #15039 ) ;
#11199 = ORIENTED_EDGE ( 'NONE', *, *, #5645, .T. ) ;
#11200 = CARTESIAN_POINT ( 'NONE',  ( -0.5636800770127728955, -4.293361309317330843, -3.531542292954304774 ) ) ;
#11201 = ORIENTED_EDGE ( 'NONE', *, *, #1289, .T. ) ;
#11202 = STYLED_ITEM ( 'NONE', ( #13533 ), #8964 ) ;
#11203 = DIRECTION ( 'NONE',  ( 0.000000000000000000, 0.000000000000000000, 1.000000000000000000 ) ) ;
#11204 = CARTESIAN_POINT ( 'NONE',  ( -31.47058823529412663, 102.2673069760056563, 10.99999999999999645 ) ) ;
#11205 = CARTESIAN_POINT ( 'NONE',  ( 10.54368182729040093, 106.4795995572428353, -18.98024639174784056 ) ) ;
#11206 = AXIS2_PLACEMENT_3D ( 'NONE', #11390, #9174, #13818 ) ;
#11207 = DIRECTION ( 'NONE',  ( -1.000000000000000000, 0.000000000000000000, 0.000000000000000000 ) ) ;
#11208 = DIRECTION ( 'NONE',  ( 0.000000000000000000, 0.000000000000000000, 1.000000000000000000 ) ) ;
#11209 = ORIENTED_EDGE ( 'NONE', *, *, #9815, .F. ) ;
#11210 = EDGE_LOOP ( 'NONE', ( #12071, #704, #12817, #13102, #11075 ) ) ;
#11211 = VERTEX_POINT ( 'NONE', #10562 ) ;
#11212 = DIRECTION ( 'NONE',  ( 0.2941176470588237613, -0.9557692240748189016, 0.000000000000000000 ) ) ;
#11213 = CARTESIAN_POINT ( 'NONE',  ( 22.05882352941176094, 71.68269180561141241, -23.50000000000000000 ) ) ;
#11214 = LINE ( 'NONE', #818, #1791 ) ;
#11215 = EDGE_LOOP ( 'NONE', ( #11331, #9183, #189, #3729 ) ) ;
#11216 = EDGE_CURVE ( 'NONE', #2876, #7167, #11634, .T. ) ;
#11217 = ADVANCED_FACE ( 'NONE', ( #7129 ), #14056, .T. ) ;
#11218 = AXIS2_PLACEMENT_3D ( 'NONE', #10806, #2608, #14230 ) ;
#11219 = ORIENTED_EDGE ( 'NONE', *, *, #14530, .T. ) ;
#11220 = ORIENTED_EDGE ( 'NONE', *, *, #3543, .T. ) ;
#11221 = EDGE_CURVE ( 'NONE', #5777, #5446, #534, .T. ) ;
#11222 = CARTESIAN_POINT ( 'NONE',  ( -33.49014761921589667, 11.74264578624790190, -25.50000000000000355 ) ) ;
#11223 = AXIS2_PLACEMENT_3D ( 'NONE', #12045, #4821, #2543 ) ;
#11224 = CARTESIAN_POINT ( 'NONE',  ( 0.000000000000000000, 0.000000000000000000, 8.000000000000000000 ) ) ;
#11225 = FILL_AREA_STYLE_COLOUR ( '', #13343 ) ;
#11226 = DIRECTION ( 'NONE',  ( 0.000000000000000000, 0.000000000000000000, 1.000000000000000000 ) ) ;
#11227 = EDGE_CURVE ( 'NONE', #5499, #9159, #7866, .T. ) ;
#11228 = ORIENTED_EDGE ( 'NONE', *, *, #1657, .F. ) ;
#11229 = FACE_BOUND ( 'NONE', #13894, .T. ) ;
#11230 = DIRECTION ( 'NONE',  ( 0.000000000000000000, 0.000000000000000000, 1.000000000000000000 ) ) ;
#11231 = AXIS2_PLACEMENT_3D ( 'NONE', #10564, #14980, #7975 ) ;
#11232 = ORIENTED_EDGE ( 'NONE', *, *, #7958, .T. ) ;
#11233 = DIRECTION ( 'NONE',  ( 1.000000000000000000, 0.000000000000000000, 0.000000000000000000 ) ) ;
#11234 = VERTEX_POINT ( 'NONE', #3813 ) ;
#11235 = AXIS2_PLACEMENT_3D ( 'NONE', #3824, #14066, #7292 ) ;
#11236 = EDGE_CURVE ( 'NONE', #14062, #8423, #3273, .T. ) ;
#11237 = ORIENTED_EDGE ( 'NONE', *, *, #7115, .T. ) ;
#11238 = CARTESIAN_POINT ( 'NONE',  ( -30.80502811811232888, -49.00442420935981147, -8.000000000000000000 ) ) ;
#11239 = AXIS2_PLACEMENT_3D ( 'NONE', #5172, #9789, #12090 ) ;
#11240 = DIRECTION ( 'NONE',  ( 1.000000000000000000, 9.237055564881302416E-14, 0.000000000000000000 ) ) ;
#11241 = VECTOR ( 'NONE', #12277, 1000.000000000000000 ) ;
#11242 = CARTESIAN_POINT ( 'NONE',  ( 0.000000000000000000, 0.000000000000000000, -45.50000000000000000 ) ) ;
#11243 = DIRECTION ( 'NONE',  ( -0.000000000000000000, -0.000000000000000000, 1.000000000000000000 ) ) ;
#11244 = CARTESIAN_POINT ( 'NONE',  ( 2.500000000000002220, 2.357898499370430834, -6.938893903907228378E-15 ) ) ;
#11245 = AXIS2_PLACEMENT_3D ( 'NONE', #10330, #14032, #13590 ) ;
#11246 = EDGE_LOOP ( 'NONE', ( #10197, #3368, #1421, #6723, #12104, #12297, #4105, #8746, #10419 ) ) ;
#11247 = CARTESIAN_POINT ( 'NONE',  ( -12.86891638962156215, 56.43380494353993271, -13.00000000000000178 ) ) ;
#11248 = CARTESIAN_POINT ( 'NONE',  ( -2.100000000000000089, 2.571758278209441957E-16, -5.000000000000000888 ) ) ;
#11249 = DIRECTION ( 'NONE',  ( 1.000000000000000000, 0.000000000000000000, 0.000000000000000000 ) ) ;
#11250 = CIRCLE ( 'NONE', #2504, 56.99999999999999289 ) ;
#11251 = ORIENTED_EDGE ( 'NONE', *, *, #6372, .T. ) ;
#11252 = DIRECTION ( 'NONE',  ( 1.000000000000000000, 0.000000000000000000, 0.000000000000000000 ) ) ;
#11253 = DIRECTION ( 'NONE',  ( -1.000000000000000000, 0.000000000000000000, 0.000000000000000000 ) ) ;
#11254 = EDGE_LOOP ( 'NONE', ( #9755, #4316, #5783, #3629 ) ) ;
#11255 = CARTESIAN_POINT ( 'NONE',  ( -9.706953719245875689, -57.06275842387046993, -10.50000000000000000 ) ) ;
#11256 = CIRCLE ( 'NONE', #1319, 3.000000000000002665 ) ;
#11257 = PLANE ( 'NONE',  #611 ) ;
#11258 = PLANE ( 'NONE',  #2189 ) ;
#11259 = EDGE_CURVE ( 'NONE', #1589, #13568, #3880, .T. ) ;
#11260 = CARTESIAN_POINT ( 'NONE',  ( 45.83364790889049090, -29.49928053175916887, 8.000000000000000000 ) ) ;
#11261 = VECTOR ( 'NONE', #9794, 1000.000000000000000 ) ;
#11262 = AXIS2_PLACEMENT_3D ( 'NONE', #1877, #2030, #2106 ) ;
#11263 = AXIS2_PLACEMENT_3D ( 'NONE', #13981, #1292, #11416 ) ;
#11264 = CARTESIAN_POINT ( 'NONE',  ( 45.96504489226007450, -23.50071946824056823, -13.00000000000000178 ) ) ;
#11265 = DIRECTION ( 'NONE',  ( 1.000000000000000000, 0.000000000000000000, 0.000000000000000000 ) ) ;
#11266 = DIRECTION ( 'NONE',  ( -0.000000000000000000, -1.000000000000000000, -0.000000000000000000 ) ) ;
#11267 = ORIENTED_EDGE ( 'NONE', *, *, #1294, .F. ) ;
#11268 = DIRECTION ( 'NONE',  ( 0.000000000000000000, 0.000000000000000000, -1.000000000000000000 ) ) ;
#11269 = CARTESIAN_POINT ( 'NONE',  ( -68.58935777509570642, -68.58935777509452691, -8.000000000000000000 ) ) ;
#11270 = AXIS2_PLACEMENT_3D ( 'NONE', #6620, #1654, #6258 ) ;
#11271 = AXIS2_PLACEMENT_3D ( 'NONE', #11988, #8689, #13114 ) ;
#11272 = CARTESIAN_POINT ( 'NONE',  ( 3.999999999999998224, -1.700175430507268937, -3.320327275037804782 ) ) ;
#11273 = AXIS2_PLACEMENT_3D ( 'NONE', #5676, #13739, #9239 ) ;
#11274 = AXIS2_PLACEMENT_3D ( 'NONE', #5148, #1586, #1429 ) ;
#11275 = DIRECTION ( 'NONE',  ( 0.000000000000000000, 0.000000000000000000, 1.000000000000000000 ) ) ;
#11276 = ORIENTED_EDGE ( 'NONE', *, *, #13823, .T. ) ;
#11277 = CARTESIAN_POINT ( 'NONE',  ( 49.57224306869054686, -6.526309611002390376, 8.000000000000000000 ) ) ;
#11278 = EDGE_LOOP ( 'NONE', ( #12803, #357 ) ) ;
#11279 = FACE_OUTER_BOUND ( 'NONE', #1618, .T. ) ;
#11280 = EDGE_CURVE ( 'NONE', #14497, #218, #5213, .T. ) ;
#11281 = DIRECTION ( 'NONE',  ( -1.000000000000000000, 0.000000000000000000, 0.000000000000000000 ) ) ;
#11282 = EDGE_CURVE ( 'NONE', #1593, #14956, #9629, .T. ) ;
#11283 = ORIENTED_EDGE ( 'NONE', *, *, #13735, .T. ) ;
#11284 = AXIS2_PLACEMENT_3D ( 'NONE', #10836, #4298, #6335 ) ;
#11285 = FACE_OUTER_BOUND ( 'NONE', #14653, .T. ) ;
#11286 = DIRECTION ( 'NONE',  ( 1.000000000000000000, 0.000000000000000000, 0.000000000000000000 ) ) ;
#11287 = SHAPE_DEFINITION_REPRESENTATION ( #1026, #5964 ) ;
#11288 = VERTEX_POINT ( 'NONE', #14429 ) ;
#11289 = CIRCLE ( 'NONE', #10299, 75.00000000000001421 ) ;
#11290 = AXIS2_PLACEMENT_3D ( 'NONE', #3986, #8601, #2843 ) ;
#11291 = AXIS2_PLACEMENT_3D ( 'NONE', #7904, #1908, #2137 ) ;
#11292 = ORIENTED_EDGE ( 'NONE', *, *, #8981, .F. ) ;
#11293 = CARTESIAN_POINT ( 'NONE',  ( -19.68583958711381854, -30.74264578624812927, 14.49999999999999822 ) ) ;
#11294 = DIRECTION ( 'NONE',  ( -1.000000000000000000, -1.387778780781443624E-14, 0.000000000000000000 ) ) ;
#11295 = DIRECTION ( 'NONE',  ( -0.000000000000000000, -0.000000000000000000, 1.000000000000000000 ) ) ;
#11296 = VERTEX_POINT ( 'NONE', #2738 ) ;
#11297 = CIRCLE ( 'NONE', #9093, 3.000000000000002665 ) ;
#11298 = ORIENTED_EDGE ( 'NONE', *, *, #1944, .F. ) ;
#11299 = AXIS2_PLACEMENT_3D ( 'NONE', #6065, #10709, #4948 ) ;
#11300 = EDGE_LOOP ( 'NONE', ( #9602, #429, #13454, #8087, #5254, #1570, #5106, #2832, #8341 ) ) ;
#11301 = CARTESIAN_POINT ( 'NONE',  ( 7.417888187663120192, 52.54657765281190507, 10.49999999999999822 ) ) ;
#11302 = CARTESIAN_POINT ( 'NONE',  ( 32.46576781417953583, -41.59008834022656487, -10.50000000000000000 ) ) ;
#11303 = DIRECTION ( 'NONE',  ( -1.000000000000000000, 0.000000000000000000, 0.000000000000000000 ) ) ;
#11304 = CYLINDRICAL_SURFACE ( 'NONE', #10978, 20.00000000000000000 ) ;
#11305 = AXIS2_PLACEMENT_3D ( 'NONE', #6186, #10751, #2625 ) ;
#11306 = AXIS2_PLACEMENT_3D ( 'NONE', #6582, #985, #9015 ) ;
#11307 = EDGE_LOOP ( 'NONE', ( #9790, #5800, #175, #12031, #8870, #580, #3548, #712, #10579 ) ) ;
#11308 = FACE_OUTER_BOUND ( 'NONE', #9829, .T. ) ;
#11309 = CARTESIAN_POINT ( 'NONE',  ( -32.10455955028197650, 102.0624585623582021, 13.51511155787192031 ) ) ;
#11310 = EDGE_CURVE ( 'NONE', #4446, #4839, #7133, .T. ) ;
#11311 = VERTEX_POINT ( 'NONE', #2880 ) ;
#11312 = DIRECTION ( 'NONE',  ( -1.000000000000000000, 0.000000000000000000, 0.000000000000000000 ) ) ;
#11313 = EDGE_CURVE ( 'NONE', #12813, #1620, #12973, .T. ) ;
#11314 = ORIENTED_EDGE ( 'NONE', *, *, #5838, .F. ) ;
#11315 = VERTEX_POINT ( 'NONE', #1748 ) ;
#11316 = CARTESIAN_POINT ( 'NONE',  ( 69.16568774265594755, -71.53347797788796925, 8.000000000000000000 ) ) ;
#11317 = CIRCLE ( 'NONE', #10818, 59.50000000000000000 ) ;
#11318 = EDGE_CURVE ( 'NONE', #8099, #11582, #8497, .T. ) ;
#11319 = DIRECTION ( 'NONE',  ( 1.000000000000000000, 0.000000000000000000, 0.000000000000000000 ) ) ;
#11320 = DIRECTION ( 'NONE',  ( -1.000000000000000000, 0.000000000000000000, 0.000000000000000000 ) ) ;
#11321 = DIRECTION ( 'NONE',  ( 0.000000000000000000, 0.000000000000000000, 1.000000000000000000 ) ) ;
#11322 = LINE ( 'NONE', #10095, #13332 ) ;
#11323 = EDGE_CURVE ( 'NONE', #10864, #13229, #12266, .T. ) ;
#11324 = DIRECTION ( 'NONE',  ( -0.000000000000000000, -0.000000000000000000, 1.000000000000000000 ) ) ;
#11325 = EDGE_CURVE ( 'NONE', #3015, #13764, #9573, .T. ) ;
#11326 = VERTEX_POINT ( 'NONE', #13285 ) ;
#11327 = VECTOR ( 'NONE', #14356, 1000.000000000000000 ) ;
#11328 = DIRECTION ( 'NONE',  ( 1.000000000000000000, 0.000000000000000000, 0.000000000000000000 ) ) ;
#11329 = CARTESIAN_POINT ( 'NONE',  ( 42.50536573064410106, 32.06294366074510549, 10.49999999999999822 ) ) ;
#11330 = CARTESIAN_POINT ( 'NONE',  ( -36.52608637591512775, 92.55687898036946137, 8.000000000000000000 ) ) ;
#11331 = ORIENTED_EDGE ( 'NONE', *, *, #5003, .F. ) ;
#11332 = PLANE ( 'NONE',  #872 ) ;
#11333 = EDGE_CURVE ( 'NONE', #8562, #452, #380, .T. ) ;
#11334 = EDGE_LOOP ( 'NONE', ( #11401, #9462, #8035, #8755 ) ) ;
#11335 = CARTESIAN_POINT ( 'NONE',  ( 0.000000000000000000, 0.000000000000000000, -4.974599999999998801 ) ) ;
#11336 = ORIENTED_EDGE ( 'NONE', *, *, #11502, .T. ) ;
#11337 = CARTESIAN_POINT ( 'NONE',  ( -47.21331623427138879, -33.48561063518577896, 10.49999999999999822 ) ) ;
#11338 = FACE_OUTER_BOUND ( 'NONE', #1214, .T. ) ;
#11339 = CARTESIAN_POINT ( 'NONE',  ( 0.000000000000000000, 0.000000000000000000, 8.000000000000000000 ) ) ;
#11340 = DIRECTION ( 'NONE',  ( 0.000000000000000000, 0.000000000000000000, 1.000000000000000000 ) ) ;
#11341 = DIRECTION ( 'NONE',  ( 0.000000000000000000, 0.000000000000000000, 1.000000000000000000 ) ) ;
#11342 = DIRECTION ( 'NONE',  ( 0.000000000000000000, 1.000000000000000000, 0.000000000000000000 ) ) ;
#11343 = EDGE_LOOP ( 'NONE', ( #12214, #2697, #4348, #6456, #14268 ) ) ;
#11344 = CYLINDRICAL_SURFACE ( 'NONE', #2341, 3.000000000000002665 ) ;
#11345 = CARTESIAN_POINT ( 'NONE',  ( 2.649999999999987033, 38.00000000000000000, -28.00000000000000000 ) ) ;
#11346 = FACE_OUTER_BOUND ( 'NONE', #7371, .T. ) ;
#11347 = CARTESIAN_POINT ( 'NONE',  ( 97.41488903138106537, -0.2790467552935826934, -10.50000000000000000 ) ) ;
#11348 = ORIENTED_EDGE ( 'NONE', *, *, #3023, .T. ) ;
#11349 = CARTESIAN_POINT ( 'NONE',  ( 38.79014761921568777, 11.74264578624841171, 14.49999999999999822 ) ) ;
#11350 = ORIENTED_EDGE ( 'NONE', *, *, #11166, .T. ) ;
#11351 = DIRECTION ( 'NONE',  ( -1.000000000000000000, 0.000000000000000000, 0.000000000000000000 ) ) ;
#11352 = DIRECTION ( 'NONE',  ( -1.000000000000000000, 2.653106492670410595E-15, 0.000000000000000000 ) ) ;
#11353 = ORIENTED_EDGE ( 'NONE', *, *, #4130, .T. ) ;
#11354 = AXIS2_PLACEMENT_3D ( 'NONE', #6032, #9240, #10676 ) ;
#11355 = CARTESIAN_POINT ( 'NONE',  ( 12.50000000000000000, 106.2673515243510991, -15.00000000000000355 ) ) ;
#11356 = CARTESIAN_POINT ( 'NONE',  ( -1.999999999999997335, 3.464101615137752610, -3.142992957459231906 ) ) ;
#11357 = APPLICATION_PROTOCOL_DEFINITION ( 'draft international standard', 'automotive_design', 1998, #7647 ) ;
#11358 = EDGE_LOOP ( 'NONE', ( #13505, #1819, #13324, #3498 ) ) ;
#11359 = VERTEX_POINT ( 'NONE', #1526 ) ;
#11360 = ORIENTED_EDGE ( 'NONE', *, *, #7452, .F. ) ;
#11361 = EDGE_CURVE ( 'NONE', #11582, #8372, #6669, .T. ) ;
#11362 = CARTESIAN_POINT ( 'NONE',  ( 0.000000000000000000, 0.000000000000000000, 0.000000000000000000 ) ) ;
#11363 = CARTESIAN_POINT ( 'NONE',  ( 9.719110480984905820, 94.50309565249440880, 19.51732164073033715 ) ) ;
#11364 = EDGE_CURVE ( 'NONE', #5169, #11991, #139, .T. ) ;
#11365 = DIRECTION ( 'NONE',  ( -0.000000000000000000, -0.000000000000000000, 1.000000000000000000 ) ) ;
#11366 = EDGE_CURVE ( 'NONE', #11429, #6857, #11547, .T. ) ;
#11368 = ORIENTED_EDGE ( 'NONE', *, *, #7489, .T. ) ;
#11367 = EDGE_CURVE ( 'NONE', #2325, #4205, #14657, .T. ) ;
#11369 = ORIENTED_EDGE ( 'NONE', *, *, #1951, .F. ) ;
#11370 = EDGE_CURVE ( 'NONE', #10704, #1787, #14694, .T. ) ;
#11371 = VERTEX_POINT ( 'NONE', #9560 ) ;
#11372 = PLANE ( 'NONE',  #9070 ) ;
#11373 = ADVANCED_FACE ( 'NONE', ( #5024 ), #9776, .F. ) ;
#11374 = DIRECTION ( 'NONE',  ( 1.000000000000000000, 0.000000000000000000, 0.000000000000000000 ) ) ;
#11375 = CARTESIAN_POINT ( 'NONE',  ( 13.71740939043365337, -51.19406879332061067, 8.000000000000000000 ) ) ;
#11376 = LINE ( 'NONE', #14790, #1767 ) ;
#11377 = ORIENTED_EDGE ( 'NONE', *, *, #4408, .T. ) ;
#11378 = CARTESIAN_POINT ( 'NONE',  ( -3.492805317593278058, 46.55633131742322917, -10.50000000000000000 ) ) ;
#11379 = ORIENTED_EDGE ( 'NONE', *, *, #13638, .F. ) ;
#11380 = ORIENTED_EDGE ( 'NONE', *, *, #9314, .T. ) ;
#11381 = LINE ( 'NONE', #2968, #12073 ) ;
#11382 = ADVANCED_FACE ( 'NONE', ( #3046 ), #10247, .F. ) ;
#11383 = ORIENTED_EDGE ( 'NONE', *, *, #14833, .T. ) ;
#11384 = EDGE_LOOP ( 'NONE', ( #10028, #14631, #6708, #6615 ) ) ;
#11385 = DIRECTION ( 'NONE',  ( 0.000000000000000000, 0.000000000000000000, 1.000000000000000000 ) ) ;
#11386 = VERTEX_POINT ( 'NONE', #5470 ) ;
#11387 = ORIENTED_EDGE ( 'NONE', *, *, #2903, .T. ) ;
#11388 = CARTESIAN_POINT ( 'NONE',  ( -52.54657765281192638, 6.917888187662934563, -8.000000000000000000 ) ) ;
#11389 = CIRCLE ( 'NONE', #6755, 3.000000000000002665 ) ;
#11390 = CARTESIAN_POINT ( 'NONE',  ( 12.86891638962116247, -56.43380494354001087, 8.000000000000000000 ) ) ;
#11391 = CARTESIAN_POINT ( 'NONE',  ( 40.12029293941316155, -89.61631465359504034, -13.00000000000000178 ) ) ;
#11392 = FACE_OUTER_BOUND ( 'NONE', #2166, .T. ) ;
#11393 = FACE_OUTER_BOUND ( 'NONE', #8626, .T. ) ;
#11394 = ORIENTED_EDGE ( 'NONE', *, *, #2118, .F. ) ;
#11395 = DIRECTION ( 'NONE',  ( 1.000000000000000000, 0.000000000000000000, 0.000000000000000000 ) ) ;
#11396 = AXIS2_PLACEMENT_3D ( 'NONE', #4854, #13210, #6270 ) ;
#11397 = CARTESIAN_POINT ( 'NONE',  ( 0.000000000000000000, 0.000000000000000000, 25.99999999999999645 ) ) ;
#11398 = AXIS2_PLACEMENT_3D ( 'NONE', #14967, #1150, #8475 ) ;
#11399 = DIRECTION ( 'NONE',  ( -0.000000000000000000, -0.000000000000000000, -1.000000000000000000 ) ) ;
#11400 = CIRCLE ( 'NONE', #11890, 3.000000000000002665 ) ;
#11401 = ORIENTED_EDGE ( 'NONE', *, *, #225, .F. ) ;
#11402 = CARTESIAN_POINT ( 'NONE',  ( 69.08004447556065486, 68.68541276968852571, -13.00000000000000178 ) ) ;
#11403 = ADVANCED_FACE ( 'NONE', ( #13581 ), #14661, .F. ) ;
#11404 = DIRECTION ( 'NONE',  ( 0.000000000000000000, 0.000000000000000000, -1.000000000000000000 ) ) ;
#11405 = ADVANCED_FACE ( 'NONE', ( #1894, #1969 ), #4335, .F. ) ;
#11406 = CARTESIAN_POINT ( 'NONE',  ( -11.45661564179884628, 61.94983405580221358, 18.07016506142803891 ) ) ;
#11407 = VECTOR ( 'NONE', #3033, 1000.000000000000000 ) ;
#11408 = EDGE_CURVE ( 'NONE', #219, #11737, #12029, .T. ) ;
#11409 = DIRECTION ( 'NONE',  ( 0.000000000000000000, 0.000000000000000000, 1.000000000000000000 ) ) ;
#11411 = DIRECTION ( 'NONE',  ( 0.000000000000000000, 0.000000000000000000, -1.000000000000000000 ) ) ;
#11410 = AXIS2_PLACEMENT_3D ( 'NONE', #14231, #3831, #8449 ) ;
#11412 = CARTESIAN_POINT ( 'NONE',  ( -31.47058823529412663, 102.2673069760056563, -79.80561291909842225 ) ) ;
#11413 = AXIS2_PLACEMENT_3D ( 'NONE', #2531, #1247, #12857 ) ;
#11414 = CARTESIAN_POINT ( 'NONE',  ( 38.79014761921569487, 11.74264578624841171, -25.50000000000000355 ) ) ;
#11416 = DIRECTION ( 'NONE',  ( -0.9557692240748183465, 0.2941176470588252045, 0.000000000000000000 ) ) ;
#11415 = PRESENTATION_LAYER_ASSIGNMENT (  '', '', ( #13589 ) ) ;
#11417 = EDGE_CURVE ( 'NONE', #10986, #303, #12988, .T. ) ;
#11418 = DIRECTION ( 'NONE',  ( 0.000000000000000000, 0.000000000000000000, 1.000000000000000000 ) ) ;
#11419 = ORIENTED_EDGE ( 'NONE', *, *, #4574, .F. ) ;
#11420 = CARTESIAN_POINT ( 'NONE',  ( 2.500000000000000888, 3.061616997868384127E-16, -4.974599999999998801 ) ) ;
#11421 = DIRECTION ( 'NONE',  ( 1.000000000000000000, 0.000000000000000000, 0.000000000000000000 ) ) ;
#11422 = CIRCLE ( 'NONE', #743, 0.5000000000000004441 ) ;
#11423 = DIRECTION ( 'NONE',  ( 0.000000000000000000, 0.000000000000000000, 1.000000000000000000 ) ) ;
#11424 = AXIS2_PLACEMENT_3D ( 'NONE', #7356, #5165, #3656 ) ;
#11425 = CARTESIAN_POINT ( 'NONE',  ( -89.61631465359519666, -37.12029293941281338, -10.50000000000000000 ) ) ;
#11426 = AXIS2_PLACEMENT_3D ( 'NONE', #5694, #6743, #9113 ) ;
#11427 = EDGE_CURVE ( 'NONE', #23, #11288, #2077, .T. ) ;
#11428 = AXIS2_PLACEMENT_3D ( 'NONE', #4067, #7538, #2773 ) ;
#11429 = VERTEX_POINT ( 'NONE', #6585 ) ;
#11430 = LINE ( 'NONE', #882, #10460 ) ;
#11431 = EDGE_LOOP ( 'NONE', ( #632, #202, #12394, #4638 ) ) ;
#11432 = DIRECTION ( 'NONE',  ( 0.000000000000000000, 0.000000000000000000, -1.000000000000000000 ) ) ;
#11433 = DIRECTION ( 'NONE',  ( -1.000000000000000000, 0.000000000000000000, 0.000000000000000000 ) ) ;
#11434 = AXIS2_PLACEMENT_3D ( 'NONE', #11927, #14199, #4022 ) ;
#11435 = AXIS2_PLACEMENT_3D ( 'NONE', #9390, #10540, #3796 ) ;
#11436 = CARTESIAN_POINT ( 'NONE',  ( 9.104688129943030006, 106.6120509519917192, -19.73833377876427519 ) ) ;
#11437 = DIRECTION ( 'NONE',  ( 1.000000000000000000, 1.778456000581264310E-15, 0.000000000000000000 ) ) ;
#11438 = EDGE_LOOP ( 'NONE', ( #12527, #7083, #14862, #10065 ) ) ;
#11439 = VECTOR ( 'NONE', #4102, 1000.000000000000000 ) ;
#11440 = ORIENTED_EDGE ( 'NONE', *, *, #14748, .T. ) ;
#11441 = ORIENTED_EDGE ( 'NONE', *, *, #3201, .T. ) ;
#11442 = CONICAL_SURFACE ( 'NONE', #525, 2.059999999999998721, 0.9599310885968738161 ) ;
#11443 = CARTESIAN_POINT ( 'NONE',  ( 6.917888187663118416, 52.54657765281190507, -13.00000000000000178 ) ) ;
#11444 = DIRECTION ( 'NONE',  ( 0.000000000000000000, 0.000000000000000000, 1.000000000000000000 ) ) ;
#11445 = PLANE ( 'NONE',  #11706 ) ;
#11446 = EDGE_LOOP ( 'NONE', ( #14708, #14800, #11383, #2100 ) ) ;
#11447 = CIRCLE ( 'NONE', #764, 0.5000000000000004441 ) ;
#11448 = ORIENTED_EDGE ( 'NONE', *, *, #3186, .T. ) ;
#11449 = VERTEX_POINT ( 'NONE', #13509 ) ;
#11450 = AXIS2_PLACEMENT_3D ( 'NONE', #10244, #6812, #14884 ) ;
#11451 = CARTESIAN_POINT ( 'NONE',  ( 8.635752201752492141, 74.50170565226535757, 19.87768552833457392 ) ) ;
#11452 = PRODUCT ( 'brake caliper housing', 'brake caliper housing', '', ( #7056 ) ) ;
#11453 = DIRECTION ( 'NONE',  ( -1.000000000000000000, 0.000000000000000000, 0.000000000000000000 ) ) ;
#11454 = CARTESIAN_POINT ( 'NONE',  ( 92.55687898036906347, 36.52608637591612961, -8.000000000000000000 ) ) ;
#11455 =( NAMED_UNIT ( * ) PLANE_ANGLE_UNIT ( ) SI_UNIT ( $, .RADIAN. ) );
#11456 = ADVANCED_FACE ( 'NONE', ( #6506 ), #2553, .T. ) ;
#11457 = DIRECTION ( 'NONE',  ( 1.000000000000000000, 0.000000000000000000, 0.000000000000000000 ) ) ;
#11458 = EDGE_CURVE ( 'NONE', #7611, #10669, #9021, .T. ) ;
#11459 = EDGE_LOOP ( 'NONE', ( #3714, #730, #465, #5183 ) ) ;
#11460 = AXIS2_PLACEMENT_3D ( 'NONE', #13245, #2840, #3981 ) ;
#11461 = LINE ( 'NONE', #3327, #14585 ) ;
#11462 = ORIENTED_EDGE ( 'NONE', *, *, #225, .T. ) ;
#11463 = DIRECTION ( 'NONE',  ( 1.000000000000000000, 0.000000000000000000, 0.000000000000000000 ) ) ;
#11464 = ORIENTED_EDGE ( 'NONE', *, *, #1001, .F. ) ;
#11465 = AXIS2_PLACEMENT_3D ( 'NONE', #7955, #12533, #14963 ) ;
#11466 = VERTEX_POINT ( 'NONE', #3265 ) ;
#11467 = ORIENTED_EDGE ( 'NONE', *, *, #1728, .F. ) ;
#11468 = CARTESIAN_POINT ( 'NONE',  ( -4.101948962586058123, 2.368261337751160767, -3.681124513963740075 ) ) ;
#11469 = VERTEX_POINT ( 'NONE', #766 ) ;
#11470 = ORIENTED_EDGE ( 'NONE', *, *, #171, .F. ) ;
#11471 = PLANE ( 'NONE',  #2197 ) ;
#11472 = CARTESIAN_POINT ( 'NONE',  ( 56.43380494353997534, 12.86891638962136319, 8.000000000000000000 ) ) ;
#11473 = AXIS2_PLACEMENT_3D ( 'NONE', #11808, #1403, #6011 ) ;
#11474 = CYLINDRICAL_SURFACE ( 'NONE', #10798, 3.000000000000002665 ) ;
#11475 = CARTESIAN_POINT ( 'NONE',  ( 19.68583958711426263, -30.74264578624780597, -28.00000000000000000 ) ) ;
#11476 = EDGE_CURVE ( 'NONE', #11873, #4338, #8095, .T. ) ;
#11477 = EDGE_CURVE ( 'NONE', #3464, #9394, #12712, .T. ) ;
#11478 = CARTESIAN_POINT ( 'NONE',  ( 3.000000000000004885, -97.00000000000000000, 8.000000000000000000 ) ) ;
#11479 = EDGE_LOOP ( 'NONE', ( #2234, #11051, #5578, #156, #13148 ) ) ;
#11480 = DIRECTION ( 'NONE',  ( 1.000000000000000000, 0.000000000000000000, 0.000000000000000000 ) ) ;
#11481 = ORIENTED_EDGE ( 'NONE', *, *, #1834, .T. ) ;
#11482 = AXIS2_PLACEMENT_3D ( 'NONE', #2078, #95, #6694 ) ;
#11483 = DIRECTION ( 'NONE',  ( -0.000000000000000000, -0.000000000000000000, 1.000000000000000000 ) ) ;
#11484 = CARTESIAN_POINT ( 'NONE',  ( 2.500000000000002220, -1.178949249685208533, 2.042000000000002036 ) ) ;
#11485 = CIRCLE ( 'NONE', #11239, 0.5000000000000004441 ) ;
#11486 = ORIENTED_EDGE ( 'NONE', *, *, #10332, .T. ) ;
#11487 = DIRECTION ( 'NONE',  ( 0.000000000000000000, 0.000000000000000000, 1.000000000000000000 ) ) ;
#11488 = EDGE_LOOP ( 'NONE', ( #2074, #4596, #3755, #5034 ) ) ;
#11489 = CIRCLE ( 'NONE', #1538, 0.5000000000000022204 ) ;
#11490 = CARTESIAN_POINT ( 'NONE',  ( 0.000000000000000000, 0.000000000000000000, -16.00000000000000000 ) ) ;
#11491 = CARTESIAN_POINT ( 'NONE',  ( -56.43380494354004639, -12.86891638962099549, 10.49999999999999822 ) ) ;
#11492 = CIRCLE ( 'NONE', #11978, 3.000000000000002665 ) ;
#11493 = DIRECTION ( 'NONE',  ( 0.000000000000000000, -0.8660254037844388186, -0.4999999999999998335 ) ) ;
#11494 = CARTESIAN_POINT ( 'NONE',  ( -7.500000000000000888, 106.7368258849775202, 20.00000000000000355 ) ) ;
#11495 = DIRECTION ( 'NONE',  ( -0.000000000000000000, -0.000000000000000000, -1.000000000000000000 ) ) ;
#11496 = CARTESIAN_POINT ( 'NONE',  ( -3.999999999999998224, -2.512220745329311722, -3.469390707569720789 ) ) ;
#11497 = ADVANCED_FACE ( 'NONE', ( #11089 ), #5394, .F. ) ;
#11498 = CARTESIAN_POINT ( 'NONE',  ( 15.88467684210547226, -49.11971303961683333, -13.00000000000000178 ) ) ;
#11499 = ADVANCED_FACE ( 'NONE', ( #5538 ), #13664, .F. ) ;
#11500 = CIRCLE ( 'NONE', #8556, 0.5000000000000004441 ) ;
#11501 = ORIENTED_EDGE ( 'NONE', *, *, #10424, .T. ) ;
#11502 = EDGE_CURVE ( 'NONE', #6680, #10072, #6735, .T. ) ;
#11503 = CARTESIAN_POINT ( 'NONE',  ( 45.83364790889049090, -29.49928053175917242, -8.000000000000000000 ) ) ;
#11504 = CARTESIAN_POINT ( 'NONE',  ( -2.682243648011669368, -3.070208061305315983, -0.04852650426602034966 ) ) ;
#11505 = EDGE_CURVE ( 'NONE', #6495, #9656, #6414, .T. ) ;
#11506 = CARTESIAN_POINT ( 'NONE',  ( 87.95718916809192933, -34.62083247296232713, 8.000000000000000000 ) ) ;
#11507 = B_SPLINE_CURVE_WITH_KNOTS ( 'NONE', 3,
 ( #10106, #8728, #5321, #6595, #5482, #11024, #629, #9948, #12167, #857, #8658, #3970, #8582, #7510, #2891, #13375, #777, #6516, #7595, #2829 ),
 .UNSPECIFIED., .F., .F.,
 ( 4, 2, 2, 2, 2, 2, 2, 2, 2, 4 ),
 ( 0.000000000000000000, 0.0009765940263104426564, 0.001464891039465661274, 0.001953188052620879675, 0.002929782078931332957, 0.003906376105241786238, 0.004882970131552239086, 0.005859564157862691934, 0.006836158184173144782, 0.007812752210483598497 ),
 .UNSPECIFIED. ) ;
#11508 = DIRECTION ( 'NONE',  ( 0.000000000000000000, 0.000000000000000000, 1.000000000000000000 ) ) ;
#11509 = EDGE_LOOP ( 'NONE', ( #13760, #7364, #8957, #6296 ) ) ;
#11510 = CIRCLE ( 'NONE', #9065, 2.649999999999985700 ) ;
#11511 = AXIS2_PLACEMENT_3D ( 'NONE', #13597, #14749, #13453 ) ;
#11512 = EDGE_CURVE ( 'NONE', #9830, #13811, #4189, .T. ) ;
#11513 = DIRECTION ( 'NONE',  ( 0.000000000000000000, 0.000000000000000000, 1.000000000000000000 ) ) ;
#11514 = AXIS2_PLACEMENT_3D ( 'NONE', #2610, #8304, #3832 ) ;
#11515 = ORIENTED_EDGE ( 'NONE', *, *, #13917, .F. ) ;
#11516 = CARTESIAN_POINT ( 'NONE',  ( -89.12622059913283579, -37.21932736666236963, -10.50000000000000000 ) ) ;
#11517 = DIRECTION ( 'NONE',  ( -1.000000000000000000, 0.000000000000000000, 0.000000000000000000 ) ) ;
#11518 = FACE_OUTER_BOUND ( 'NONE', #6093, .T. ) ;
#11519 = ORIENTED_EDGE ( 'NONE', *, *, #13805, .T. ) ;
#11520 = EDGE_CURVE ( 'NONE', #4183, #10362, #9339, .T. ) ;
#11521 = ORIENTED_EDGE ( 'NONE', *, *, #1846, .F. ) ;
#11522 = ORIENTED_EDGE ( 'NONE', *, *, #3965, .T. ) ;
#11523 = EDGE_CURVE ( 'NONE', #12160, #5971, #10959, .T. ) ;
#11524 = AXIS2_PLACEMENT_3D ( 'NONE', #2933, #5138, #6189 ) ;
#11525 = VERTEX_POINT ( 'NONE', #7110 ) ;
#11526 = CIRCLE ( 'NONE', #4965, 95.00000000000001421 ) ;
#11527 = FACE_OUTER_BOUND ( 'NONE', #13878, .T. ) ;
#11528 = DIRECTION ( 'NONE',  ( 0.000000000000000000, 0.000000000000000000, -1.000000000000000000 ) ) ;
#11529 = AXIS2_PLACEMENT_3D ( 'NONE', #6869, #8015, #8168 ) ;
#11530 = CARTESIAN_POINT ( 'NONE',  ( 0.000000000000000000, 0.000000000000000000, 13.00000000000000178 ) ) ;
#11531 = EDGE_LOOP ( 'NONE', ( #8854, #10501, #7334, #11992 ) ) ;
#11532 = VERTEX_POINT ( 'NONE', #3637 ) ;
#11533 = AXIS2_PLACEMENT_3D ( 'NONE', #1283, #8181, #10760 ) ;
#11534 = ORIENTED_EDGE ( 'NONE', *, *, #14238, .F. ) ;
#11535 = CIRCLE ( 'NONE', #12733, 17.00000000000000711 ) ;
#11536 = AXIS2_PLACEMENT_3D ( 'NONE', #6116, #3843, #5204 ) ;
#11537 = CARTESIAN_POINT ( 'NONE',  ( 68.58935777509475429, -68.58935777509547904, -8.000000000000000000 ) ) ;
#11538 = FACE_OUTER_BOUND ( 'NONE', #1371, .T. ) ;
#11539 = FACE_OUTER_BOUND ( 'NONE', #11589, .T. ) ;
#11540 = DIRECTION ( 'NONE',  ( 0.000000000000000000, 0.000000000000000000, 1.000000000000000000 ) ) ;
#11541 = EDGE_LOOP ( 'NONE', ( #1559, #9500, #6479, #11467 ) ) ;
#11542 = DIRECTION ( 'NONE',  ( -1.000000000000000000, 0.000000000000000000, 0.000000000000000000 ) ) ;
#11543 = ORIENTED_EDGE ( 'NONE', *, *, #10451, .F. ) ;
#11544 = FACE_OUTER_BOUND ( 'NONE', #13111, .T. ) ;
#11545 = DIRECTION ( 'NONE',  ( 1.000000000000000000, 0.000000000000000000, 0.000000000000000000 ) ) ;
#11546 = VERTEX_POINT ( 'NONE', #9251 ) ;
#11547 = CIRCLE ( 'NONE', #620, 3.000000000000002665 ) ;
#11548 = VERTEX_POINT ( 'NONE', #1147 ) ;
#11549 = DIRECTION ( 'NONE',  ( 0.000000000000000000, 0.000000000000000000, -1.000000000000000000 ) ) ;
#11550 = EDGE_CURVE ( 'NONE', #14062, #12763, #3049, .T. ) ;
#11551 = VERTEX_POINT ( 'NONE', #5685 ) ;
#11552 = ORIENTED_EDGE ( 'NONE', *, *, #3013, .F. ) ;
#11553 = VECTOR ( 'NONE', #13633, 1000.000000000000000 ) ;
#11554 = DIRECTION ( 'NONE',  ( 0.000000000000000000, 0.000000000000000000, 1.000000000000000000 ) ) ;
#11555 = DIRECTION ( 'NONE',  ( -0.000000000000000000, -0.000000000000000000, -1.000000000000000000 ) ) ;
#11556 = AXIS2_PLACEMENT_3D ( 'NONE', #12450, #9098, #9246 ) ;
#11557 = FACE_OUTER_BOUND ( 'NONE', #14036, .T. ) ;
#11558 = CARTESIAN_POINT ( 'NONE',  ( 0.02448733951239540421, 4.877042772274725380, -3.751161874094022686 ) ) ;
#11559 = VERTEX_POINT ( 'NONE', #3570 ) ;
#11560 = CARTESIAN_POINT ( 'NONE',  ( -13.71740939043329277, 51.19406879332069593, -13.00000000000000178 ) ) ;
#11561 = VERTEX_POINT ( 'NONE', #8260 ) ;
#11562 = CARTESIAN_POINT ( 'NONE',  ( 70.71067811865437136, -70.71067811865513875, -8.000000000000000000 ) ) ;
#11563 = ORIENTED_EDGE ( 'NONE', *, *, #5416, .T. ) ;
#11564 = AXIS2_PLACEMENT_3D ( 'NONE', #1258, #961, #5871 ) ;
#11565 = LINE ( 'NONE', #11484, #10143 ) ;
#11566 = B_SPLINE_CURVE_WITH_KNOTS ( 'NONE', 3,
 ( #8902, #1852, #13536, #3143, #7760, #2000, #9048, #5496, #10119, #14762, #4359, #7836, #13696, #2520, #9351, #10572, #5715, #9278 ),
 .UNSPECIFIED., .F., .F.,
 ( 4, 2, 2, 2, 2, 2, 2, 2, 4 ),
 ( 0.001002887730653551817, 0.001856445934617264627, 0.002710004138580977221, 0.003563562342544689815, 0.004417120546508402842, 0.005270678750472115003, 0.006124236954435828030, 0.006977795158399540190, 0.007831353362363253218 ),
 .UNSPECIFIED. ) ;
#11567 = EDGE_CURVE ( 'NONE', #5532, #10072, #13715, .T. ) ;
#11568 = ORIENTED_EDGE ( 'NONE', *, *, #6202, .F. ) ;
#11569 = DIRECTION ( 'NONE',  ( 0.000000000000000000, 0.000000000000000000, 1.000000000000000000 ) ) ;
#11570 = ADVANCED_FACE ( 'NONE', ( #4630 ), #7956, .T. ) ;
#11571 = EDGE_CURVE ( 'NONE', #215, #6876, #6911, .T. ) ;
#11572 = VERTEX_POINT ( 'NONE', #4559 ) ;
#11573 = CARTESIAN_POINT ( 'NONE',  ( -33.48561063518626923, 47.21331623427104063, -13.00000000000000178 ) ) ;
#11574 = ORIENTED_EDGE ( 'NONE', *, *, #530, .T. ) ;
#11575 = DIRECTION ( 'NONE',  ( 0.000000000000000000, 0.000000000000000000, -1.000000000000000000 ) ) ;
#11576 = DIRECTION ( 'NONE',  ( -0.000000000000000000, -0.000000000000000000, 1.000000000000000000 ) ) ;
#11577 = DIRECTION ( 'NONE',  ( -1.000000000000000000, 0.000000000000000000, 0.000000000000000000 ) ) ;
#11578 = LINE ( 'NONE', #4510, #7754 ) ;
#11579 = CIRCLE ( 'NONE', #1387, 63.00000000000000000 ) ;
#11580 = DIRECTION ( 'NONE',  ( 1.000000000000000000, 0.000000000000000000, 0.000000000000000000 ) ) ;
#11581 = CARTESIAN_POINT ( 'NONE',  ( -30.80502811811232888, -49.00442420935981147, 8.000000000000000000 ) ) ;
#11582 = VERTEX_POINT ( 'NONE', #210 ) ;
#11583 = DIRECTION ( 'NONE',  ( 0.000000000000000000, 0.000000000000000000, 1.000000000000000000 ) ) ;
#11584 = DIRECTION ( 'NONE',  ( 0.000000000000000000, 0.000000000000000000, 1.000000000000000000 ) ) ;
#11585 = DIRECTION ( 'NONE',  ( 0.000000000000000000, 0.000000000000000000, -1.000000000000000000 ) ) ;
#11586 = CARTESIAN_POINT ( 'NONE',  ( -33.49014761921588956, 11.74264578624790190, -25.50000000000000355 ) ) ;
#11587 = ORIENTED_EDGE ( 'NONE', *, *, #546, .F. ) ;
#11588 = DIRECTION ( 'NONE',  ( 0.000000000000000000, 0.000000000000000000, 1.000000000000000000 ) ) ;
#11589 = EDGE_LOOP ( 'NONE', ( #7945, #11574, #10401, #1118, #804, #6487, #7157, #13556 ) ) ;
#11590 = ADVANCED_FACE ( 'NONE', ( #5759 ), #11474, .T. ) ;
#11591 = DIRECTION ( 'NONE',  ( -1.000000000000000000, 1.826024711554534012E-15, 0.000000000000000000 ) ) ;
#11592 = DIRECTION ( 'NONE',  ( -0.000000000000000000, -0.000000000000000000, -1.000000000000000000 ) ) ;
#11593 = CARTESIAN_POINT ( 'NONE',  ( -3.333333333333331705, 2.694301256218250451, -3.300726591567082480 ) ) ;
#11594 = EDGE_LOOP ( 'NONE', ( #13416, #307, #4662 ) ) ;
#11595 = CARTESIAN_POINT ( 'NONE',  ( -13.71740939043329277, 51.19406879332069593, 8.000000000000000000 ) ) ;
#11596 = DIRECTION ( 'NONE',  ( 0.000000000000000000, 0.000000000000000000, -1.000000000000000000 ) ) ;
#11597 = DIRECTION ( 'NONE',  ( -1.000000000000000000, 0.000000000000000000, 0.000000000000000000 ) ) ;
#11598 = ORIENTED_EDGE ( 'NONE', *, *, #14241, .T. ) ;
#11599 = ORIENTED_EDGE ( 'NONE', *, *, #13168, .T. ) ;
#11600 = EDGE_CURVE ( 'NONE', #10752, #10743, #2345, .T. ) ;
#11601 = ORIENTED_EDGE ( 'NONE', *, *, #14273, .F. ) ;
#11602 = EDGE_CURVE ( 'NONE', #14105, #8983, #4267, .T. ) ;
#11603 = DIRECTION ( 'NONE',  ( 0.000000000000000000, 0.000000000000000000, 1.000000000000000000 ) ) ;
#11604 = CARTESIAN_POINT ( 'NONE',  ( 66.70695371924546180, 57.06275842387054098, -13.00000000000000178 ) ) ;
#11605 = CARTESIAN_POINT ( 'NONE',  ( 26.49999999999971578, 45.89934640057541060, 8.000000000000000000 ) ) ;
#11606 = CARTESIAN_POINT ( 'NONE',  ( 25.00000000000000000, 81.24038404635960831, -23.50000000000000000 ) ) ;
#11607 = ORIENTED_EDGE ( 'NONE', *, *, #8696, .T. ) ;
#11608 = ORIENTED_EDGE ( 'NONE', *, *, #13027, .T. ) ;
#11609 = ORIENTED_EDGE ( 'NONE', *, *, #12757, .T. ) ;
#11610 = ADVANCED_FACE ( 'NONE', ( #10542 ), #4779, .F. ) ;
#11611 = PLANE ( 'NONE',  #14407 ) ;
#11612 = DIRECTION ( 'NONE',  ( 0.2941176470588243164, 0.9557692240748186796, -0.000000000000000000 ) ) ;
#11613 = ORIENTED_EDGE ( 'NONE', *, *, #722, .T. ) ;
#11614 = VERTEX_POINT ( 'NONE', #13977 ) ;
#11615 = CARTESIAN_POINT ( 'NONE',  ( 14.00000000000000000, 1.714505518806294638E-15, 14.49999999999999822 ) ) ;
#11616 = CIRCLE ( 'NONE', #8205, 59.50000000000000000 ) ;
#11617 = VERTEX_POINT ( 'NONE', #2492 ) ;
#11618 = EDGE_LOOP ( 'NONE', ( #9177, #7596, #8516, #10219 ) ) ;
#11619 = EDGE_CURVE ( 'NONE', #452, #8824, #13819, .T. ) ;
#11620 = CARTESIAN_POINT ( 'NONE',  ( 0.000000000000000000, 0.000000000000000000, 0.000000000000000000 ) ) ;
#11621 = CARTESIAN_POINT ( 'NONE',  ( 0.000000000000000000, 0.000000000000000000, -8.000000000000000000 ) ) ;
#11622 = CARTESIAN_POINT ( 'NONE',  ( 0.000000000000000000, 0.000000000000000000, -10.50000000000000000 ) ) ;
#11623 = CARTESIAN_POINT ( 'NONE',  ( 6.852625091553089298, 52.05085522212500138, -10.50000000000000000 ) ) ;
#11624 = DIRECTION ( 'NONE',  ( 0.000000000000000000, 0.000000000000000000, -1.000000000000000000 ) ) ;
#11625 = ORIENTED_EDGE ( 'NONE', *, *, #14805, .T. ) ;
#11626 =( NAMED_UNIT ( * ) PLANE_ANGLE_UNIT ( ) SI_UNIT ( $, .RADIAN. ) );
#11627 = DIRECTION ( 'NONE',  ( 0.000000000000000000, 0.000000000000000000, -1.000000000000000000 ) ) ;
#11628 = ORIENTED_EDGE ( 'NONE', *, *, #3061, .F. ) ;
#11629 = DIRECTION ( 'NONE',  ( 0.000000000000000000, 0.000000000000000000, -1.000000000000000000 ) ) ;
#11630 = AXIS2_PLACEMENT_3D ( 'NONE', #8362, #2741, #12018 ) ;
#11631 = CARTESIAN_POINT ( 'NONE',  ( 31.32121808728250656, 96.02101045561127535, 14.76552927760548073 ) ) ;
#11632 = ORIENTED_EDGE ( 'NONE', *, *, #12704, .F. ) ;
#11633 = DIRECTION ( 'NONE',  ( -1.000000000000000000, 0.000000000000000000, 0.000000000000000000 ) ) ;
#11634 = LINE ( 'NONE', #162, #8123 ) ;
#11635 = DIRECTION ( 'NONE',  ( 0.000000000000000000, 0.000000000000000000, -1.000000000000000000 ) ) ;
#11636 = DIRECTION ( 'NONE',  ( -0.000000000000000000, -0.000000000000000000, 1.000000000000000000 ) ) ;
#11637 = AXIS2_PLACEMENT_3D ( 'NONE', #13480, #5133, #660 ) ;
#11638 = ITEM_DEFINED_TRANSFORMATION ( 'NONE', 'NONE', #2652,  #5108 ) ;
#11639 = ADVANCED_FACE ( 'NONE', ( #1288 ), #6182, .T. ) ;
#11640 = AXIS2_PLACEMENT_3D ( 'NONE', #9107, #4711, #12762 ) ;
#11641 = DIRECTION ( 'NONE',  ( 1.000000000000000000, 0.000000000000000000, 0.000000000000000000 ) ) ;
#11642 = ADVANCED_FACE ( 'NONE', ( #11557 ), #1367, .T. ) ;
#11643 = ORIENTED_EDGE ( 'NONE', *, *, #3112, .F. ) ;
#11644 = DIRECTION ( 'NONE',  ( 1.000000000000000000, 0.000000000000000000, 0.000000000000000000 ) ) ;
#11645 = CARTESIAN_POINT ( 'NONE',  ( -25.00000000000000000, 81.24038404635962252, 26.00000000000000000 ) ) ;
#11646 = DIRECTION ( 'NONE',  ( -1.000000000000000000, 0.000000000000000000, 0.000000000000000000 ) ) ;
#11647 = EDGE_CURVE ( 'NONE', #7296, #5870, #4752, .T. ) ;
#11648 = AXIS2_PLACEMENT_3D ( 'NONE', #4117, #10949, #8517 ) ;
#11649 = DIRECTION ( 'NONE',  ( -1.000000000000000000, 0.000000000000000000, 0.000000000000000000 ) ) ;
#11650 = ORIENTED_EDGE ( 'NONE', *, *, #12475, .T. ) ;
#11651 = APPLICATION_CONTEXT ( 'automotive_design' ) ;
#11652 = VECTOR ( 'NONE', #5652, 1000.000000000000000 ) ;
#11653 = DIRECTION ( 'NONE',  ( 0.000000000000000000, 0.000000000000000000, 1.000000000000000000 ) ) ;
#11654 = AXIS2_PLACEMENT_3D ( 'NONE', #11957, #3756, #8447 ) ;
#11655 = ORIENTED_EDGE ( 'NONE', *, *, #3752, .T. ) ;
#11656 = AXIS2_PLACEMENT_3D ( 'NONE', #12682, #1073, #2195 ) ;
#11657 = PRODUCT_RELATED_PRODUCT_CATEGORY ( 'part', '', ( #4170 ) ) ;
#11658 = DIRECTION ( 'NONE',  ( -0.000000000000000000, -0.000000000000000000, 1.000000000000000000 ) ) ;
#11659 = CARTESIAN_POINT ( 'NONE',  ( 0.000000000000000000, 0.000000000000000000, -8.000000000000000000 ) ) ;
#11660 = CARTESIAN_POINT ( 'NONE',  ( 0.000000000000000000, 0.000000000000000000, 8.000000000000000000 ) ) ;
#11661 = CARTESIAN_POINT ( 'NONE',  ( 30.80502811811196295, 49.00442420936003174, -8.000000000000000000 ) ) ;
#11662 = EDGE_CURVE ( 'NONE', #1485, #15024, #14412, .T. ) ;
#11663 = VECTOR ( 'NONE', #5081, 1000.000000000000000 ) ;
#11664 = ORIENTED_EDGE ( 'NONE', *, *, #2686, .F. ) ;
#11665 = CARTESIAN_POINT ( 'NONE',  ( 44.13108361037843252, 56.43380494353993271, -8.000000000000000000 ) ) ;
#11666 = DIRECTION ( 'NONE',  ( -0.000000000000000000, -0.000000000000000000, 1.000000000000000000 ) ) ;
#11667 = CIRCLE ( 'NONE', #2916, 10.00000000000000178 ) ;
#11668 = LINE ( 'NONE', #265, #541 ) ;
#11669 = EDGE_LOOP ( 'NONE', ( #7781, #2282, #10800, #14835, #14861, #8619 ) ) ;
#11670 = VERTEX_POINT ( 'NONE', #12977 ) ;
#11671 = VECTOR ( 'NONE', #12020, 1000.000000000000000 ) ;
#11672 = VERTEX_POINT ( 'NONE', #3719 ) ;
#11673 = AXIS2_PLACEMENT_3D ( 'NONE', #14111, #9611, #9757 ) ;
#11674 = ORIENTED_EDGE ( 'NONE', *, *, #9033, .F. ) ;
#11675 = DIRECTION ( 'NONE',  ( 0.000000000000000000, 0.000000000000000000, -1.000000000000000000 ) ) ;
#11676 = VECTOR ( 'NONE', #11126, 1000.000000000000000 ) ;
#11677 = DIRECTION ( 'NONE',  ( 1.000000000000000000, 0.000000000000000000, 0.000000000000000000 ) ) ;
#11678 = VECTOR ( 'NONE', #6178, 1000.000000000000000 ) ;
#11679 = CARTESIAN_POINT ( 'NONE',  ( -50.00000000000000000, 0.000000000000000000, 13.00000000000000178 ) ) ;
#11680 = DIRECTION ( 'NONE',  ( 0.000000000000000000, 0.000000000000000000, 1.000000000000000000 ) ) ;
#11681 = CARTESIAN_POINT ( 'NONE',  ( 94.51066581171355097, 1.674280531758986834, 8.000000000000000000 ) ) ;
#11682 = ORIENTED_EDGE ( 'NONE', *, *, #1088, .T. ) ;
#11683 = ORIENTED_EDGE ( 'NONE', *, *, #1746, .F. ) ;
#11684 = EDGE_CURVE ( 'NONE', #13374, #11825, #6045, .T. ) ;
#11685 = CARTESIAN_POINT ( 'NONE',  ( -6.123233995736766085E-15, -100.0000000000000000, -8.000000000000000000 ) ) ;
#11687 = EDGE_CURVE ( 'NONE', #11105, #12545, #4714, .T. ) ;
#11686 = DIRECTION ( 'NONE',  ( -1.000000000000000000, 0.000000000000000000, 0.000000000000000000 ) ) ;
#11688 = AXIS2_PLACEMENT_3D ( 'NONE', #5455, #1882, #8635 ) ;
#11689 = EDGE_CURVE ( 'NONE', #12431, #2546, #2044, .T. ) ;
#11690 = VERTEX_POINT ( 'NONE', #10687 ) ;
#11691 = ORIENTED_EDGE ( 'NONE', *, *, #12185, .T. ) ;
#11692 = LINE ( 'NONE', #6958, #1366 ) ;
#11693 = EDGE_LOOP ( 'NONE', ( #3476, #1837 ) ) ;
#11694 = DIRECTION ( 'NONE',  ( 1.000000000000000000, 0.000000000000000000, 0.000000000000000000 ) ) ;
#11695 = EDGE_CURVE ( 'NONE', #12160, #7436, #7852, .T. ) ;
#11696 = DIRECTION ( 'NONE',  ( -1.000000000000000000, 0.000000000000000000, 0.000000000000000000 ) ) ;
#11697 = CIRCLE ( 'NONE', #10955, 0.5000000000000004441 ) ;
#11698 = CARTESIAN_POINT ( 'NONE',  ( 37.12029293941315444, -89.61631465359504034, 8.000000000000000000 ) ) ;
#11699 = VERTEX_POINT ( 'NONE', #6201 ) ;
#11700 = DIRECTION ( 'NONE',  ( 0.000000000000000000, 0.000000000000000000, 1.000000000000000000 ) ) ;
#11701 = DIRECTION ( 'NONE',  ( 0.000000000000000000, 0.000000000000000000, 1.000000000000000000 ) ) ;
#11702 = AXIS2_PLACEMENT_3D ( 'NONE', #2491, #10972, #11696 ) ;
#11703 = ORIENTED_EDGE ( 'NONE', *, *, #14090, .T. ) ;
#11704 = CARTESIAN_POINT ( 'NONE',  ( 13.71740939043365337, -51.19406879332061067, -13.00000000000000178 ) ) ;
#11705 = EDGE_CURVE ( 'NONE', #14140, #5547, #14703, .T. ) ;
#11706 = AXIS2_PLACEMENT_3D ( 'NONE', #12799, #5874, #1044 ) ;
#11707 = ORIENTED_EDGE ( 'NONE', *, *, #515, .T. ) ;
#11708 = DIRECTION ( 'NONE',  ( 0.000000000000000000, 0.000000000000000000, 1.000000000000000000 ) ) ;
#11709 = CARTESIAN_POINT ( 'NONE',  ( -37.12029293941250074, 89.61631465359532456, -10.50000000000000000 ) ) ;
#11710 = CIRCLE ( 'NONE', #11218, 3.000000000000002665 ) ;
#11711 = CARTESIAN_POINT ( 'NONE',  ( 2.804994570502170159, 3.229033611042449348, -3.526374918436834260 ) ) ;
#11712 = CARTESIAN_POINT ( 'NONE',  ( 2.682243648011666259, 3.070208061305303548, -0.04852650426601186340 ) ) ;
#11713 = CARTESIAN_POINT ( 'NONE',  ( -8.632958377326437116, 106.6512898904676092, 19.87266383408973525 ) ) ;
#11714 = FACE_OUTER_BOUND ( 'NONE', #14069, .T. ) ;
#11715 = DIRECTION ( 'NONE',  ( 0.000000000000000000, 0.000000000000000000, 1.000000000000000000 ) ) ;
#11716 = AXIS2_PLACEMENT_3D ( 'NONE', #8677, #799, #2001 ) ;
#11717 = LINE ( 'NONE', #11498, #14113 ) ;
#11718 = EDGE_LOOP ( 'NONE', ( #4838, #4021, #1340, #9247, #14912, #7212 ) ) ;
#11719 = DIRECTION ( 'NONE',  ( 0.000000000000000000, 0.000000000000000000, -1.000000000000000000 ) ) ;
#11720 = CARTESIAN_POINT ( 'NONE',  ( -39.61975340586620575, -91.27544013909724185, 8.000000000000000000 ) ) ;
#11721 = AXIS2_PLACEMENT_3D ( 'NONE', #3025, #7646, #9234 ) ;
#11722 = LINE ( 'NONE', #4962, #4929 ) ;
#11723 = B_SPLINE_CURVE_WITH_KNOTS ( 'NONE', 3,
 ( #1876, #672, #9997, #6645 ),
 .UNSPECIFIED., .F., .F.,
 ( 4, 4 ),
 ( 0.000000000000000000, 0.001005167940839974024 ),
 .UNSPECIFIED. ) ;
#11724 = FACE_OUTER_BOUND ( 'NONE', #288, .T. ) ;
#11725 = CIRCLE ( 'NONE', #14380, 2.649999999999993694 ) ;
#11726 = ORIENTED_EDGE ( 'NONE', *, *, #1891, .F. ) ;
#11727 = EDGE_CURVE ( 'NONE', #9073, #13137, #5068, .T. ) ;
#11728 = DIRECTION ( 'NONE',  ( 1.000000000000000000, 0.000000000000000000, 0.000000000000000000 ) ) ;
#11729 = EDGE_LOOP ( 'NONE', ( #5390, #4892, #3084, #1410, #2131 ) ) ;
#11730 = DIRECTION ( 'NONE',  ( 0.000000000000000000, 0.000000000000000000, 1.000000000000000000 ) ) ;
#11731 = DIRECTION ( 'NONE',  ( -1.000000000000000000, 0.000000000000000000, 0.000000000000000000 ) ) ;
#11732 = AXIS2_PLACEMENT_3D ( 'NONE', #1179, #13943, #1253 ) ;
#11733 = DIRECTION ( 'NONE',  ( -0.000000000000000000, -0.000000000000000000, 1.000000000000000000 ) ) ;
#11734 = DIRECTION ( 'NONE',  ( 0.000000000000000000, 0.000000000000000000, 1.000000000000000000 ) ) ;
#11735 = ORIENTED_EDGE ( 'NONE', *, *, #12903, .T. ) ;
#11736 = AXIS2_PLACEMENT_3D ( 'NONE', #4384, #1942, #10138 ) ;
#11737 = VERTEX_POINT ( 'NONE', #9760 ) ;
#11738 = CARTESIAN_POINT ( 'NONE',  ( -33.48561063518626923, 47.21331623427104063, -13.00000000000000178 ) ) ;
#11739 = DIRECTION ( 'NONE',  ( -0.000000000000000000, -0.000000000000000000, 1.000000000000000000 ) ) ;
#11740 = CARTESIAN_POINT ( 'NONE',  ( -52.54657765281192638, 6.917888187662934563, 8.000000000000000000 ) ) ;
#11741 = CIRCLE ( 'NONE', #5899, 100.0000000000000000 ) ;
#11742 = VERTEX_POINT ( 'NONE', #13050 ) ;
#11743 = CIRCLE ( 'NONE', #101, 5.560781378645573980 ) ;
#11744 = ORIENTED_EDGE ( 'NONE', *, *, #7590, .F. ) ;
#11745 = EDGE_CURVE ( 'NONE', #13021, #8628, #841, .T. ) ;
#11746 = EDGE_CURVE ( 'NONE', #11672, #14620, #13201, .T. ) ;
#11747 = ORIENTED_EDGE ( 'NONE', *, *, #11367, .T. ) ;
#11748 = DIRECTION ( 'NONE',  ( 0.000000000000000000, 0.000000000000000000, 1.000000000000000000 ) ) ;
#11749 = DIRECTION ( 'NONE',  ( 0.000000000000000000, 0.000000000000000000, 1.000000000000000000 ) ) ;
#11750 = CARTESIAN_POINT ( 'NONE',  ( 0.5636800770129354321, 4.293361309317172747, -3.531542292955333728 ) ) ;
#11751 = CIRCLE ( 'NONE', #3988, 100.0000000000000000 ) ;
#11752 = DIRECTION ( 'NONE',  ( 1.000000000000000000, 0.000000000000000000, 0.000000000000000000 ) ) ;
#11753 = LINE ( 'NONE', #10523, #8138 ) ;
#11754 = CONICAL_SURFACE ( 'NONE', #11273, 18.00000000000000355, 0.7853981633974439491 ) ;
#11755 = CARTESIAN_POINT ( 'NONE',  ( -12.34206246762915882, 94.19488728021195811, 16.27883530325393835 ) ) ;
#11756 = ORIENTED_EDGE ( 'NONE', *, *, #7871, .T. ) ;
#11757 = DIRECTION ( 'NONE',  ( -1.000000000000000000, 0.000000000000000000, 0.000000000000000000 ) ) ;
#11758 = CARTESIAN_POINT ( 'NONE',  ( 0.000000000000000000, 0.000000000000000000, -16.00000000000000000 ) ) ;
#11759 = CARTESIAN_POINT ( 'NONE',  ( -52.72775723226775568, 7.383907457638128058, -10.50000000000000000 ) ) ;
#11760 = VERTEX_POINT ( 'NONE', #3862 ) ;
#11761 = AXIS2_PLACEMENT_3D ( 'NONE', #14002, #8213, #11649 ) ;
#11762 = ORIENTED_EDGE ( 'NONE', *, *, #5636, .T. ) ;
#11763 = DIRECTION ( 'NONE',  ( -1.000000000000000000, 0.000000000000000000, 0.000000000000000000 ) ) ;
#11764 = AXIS2_PLACEMENT_3D ( 'NONE', #9454, #1646, #6253 ) ;
#11765 = AXIS2_PLACEMENT_3D ( 'NONE', #9732, #7229, #1781 ) ;
#11766 = VECTOR ( 'NONE', #11009, 1000.000000000000000 ) ;
#11767 = ORIENTED_EDGE ( 'NONE', *, *, #12150, .T. ) ;
#11768 = CARTESIAN_POINT ( 'NONE',  ( 56.43380494353997534, 12.86891638962136319, -8.000000000000000000 ) ) ;
#11769 = CARTESIAN_POINT ( 'NONE',  ( 68.58935777509475429, -68.58935777509547904, 8.000000000000000000 ) ) ;
#11770 = EDGE_CURVE ( 'NONE', #13905, #5260, #9305, .T. ) ;
#11771 = CARTESIAN_POINT ( 'NONE',  ( 37.12029293941379393, 89.61631465359479876, -13.00000000000000178 ) ) ;
#11772 = DIRECTION ( 'NONE',  ( 1.000000000000000000, 0.000000000000000000, 0.000000000000000000 ) ) ;
#11773 = CIRCLE ( 'NONE', #615, 14.00000000000000000 ) ;
#11774 = DIRECTION ( 'NONE',  ( 1.000000000000000000, 0.000000000000000000, 0.000000000000000000 ) ) ;
#11775 = CARTESIAN_POINT ( 'NONE',  ( -12.39897948556635754, 73.96800191783273704, -16.00000000000000000 ) ) ;
#11776 = ADVANCED_FACE ( 'NONE', ( #8631 ), #6445, .F. ) ;
#11777 = ORIENTED_EDGE ( 'NONE', *, *, #11361, .T. ) ;
#11778 = CARTESIAN_POINT ( 'NONE',  ( -3.999999999999996447, 2.309401076758498039, -3.433295621305378020 ) ) ;
#11779 = VECTOR ( 'NONE', #10323, 1000.000000000000227 ) ;
#11780 = ORIENTED_EDGE ( 'NONE', *, *, #8742, .T. ) ;
#11781 = DIRECTION ( 'NONE',  ( 1.000000000000000000, 0.000000000000000000, 0.000000000000000000 ) ) ;
#11782 = EDGE_LOOP ( 'NONE', ( #3258, #3616, #9421, #138, #10361 ) ) ;
#11783 = AXIS2_PLACEMENT_3D ( 'NONE', #9771, #13283, #2877 ) ;
#11784 = DIRECTION ( 'NONE',  ( -1.000000000000000000, 0.000000000000000000, 0.000000000000000000 ) ) ;
#11785 = ORIENTED_EDGE ( 'NONE', *, *, #9533, .T. ) ;
#11786 = LINE ( 'NONE', #161, #2924 ) ;
#11787 = EDGE_CURVE ( 'NONE', #13020, #11806, #9467, .T. ) ;
#11788 = ADVANCED_FACE ( 'NONE', ( #907 ), #2943, .F. ) ;
#11789 = LINE ( 'NONE', #8133, #4258 ) ;
#11790 = DIRECTION ( 'NONE',  ( 1.000000000000000000, -7.105427357601001859E-15, 0.000000000000000000 ) ) ;
#11791 = CARTESIAN_POINT ( 'NONE',  ( -2.775557561562891351E-14, -4.618802153517009401, -0.5000000000000004441 ) ) ;
#11792 = DIRECTION ( 'NONE',  ( -1.000000000000000000, 0.000000000000000000, 0.000000000000000000 ) ) ;
#11793 = VERTEX_POINT ( 'NONE', #12514 ) ;
#11794 = DIRECTION ( 'NONE',  ( -1.000000000000000000, 0.000000000000000000, 0.000000000000000000 ) ) ;
#11795 = VECTOR ( 'NONE', #9317, 1000.000000000000000 ) ;
#11796 = ORIENTED_EDGE ( 'NONE', *, *, #1832, .F. ) ;
#11797 = ADVANCED_FACE ( 'NONE', ( #8924 ), #5525, .T. ) ;
#11798 = FACE_OUTER_BOUND ( 'NONE', #224, .T. ) ;
#11799 = DIRECTION ( 'NONE',  ( -1.000000000000000000, 0.000000000000000000, 0.000000000000000000 ) ) ;
#11800 = DIRECTION ( 'NONE',  ( 1.000000000000000000, 2.664535259100375697E-15, 0.000000000000000000 ) ) ;
#11801 = DIRECTION ( 'NONE',  ( -0.5000000000000019984, -0.8660254037844375974, 0.000000000000000000 ) ) ;
#11802 = ORIENTED_EDGE ( 'NONE', *, *, #9856, .T. ) ;
#11803 = AXIS2_PLACEMENT_3D ( 'NONE', #12797, #2382, #9068 ) ;
#11804 = FACE_OUTER_BOUND ( 'NONE', #2636, .T. ) ;
#11805 = ORIENTED_EDGE ( 'NONE', *, *, #14627, .T. ) ;
#11806 = VERTEX_POINT ( 'NONE', #14787 ) ;
#11807 = DIRECTION ( 'NONE',  ( 1.000000000000000000, 0.000000000000000000, 0.000000000000000000 ) ) ;
#11808 = CARTESIAN_POINT ( 'NONE',  ( 0.000000000000000000, 0.000000000000000000, -8.000000000000000000 ) ) ;
#11809 = CARTESIAN_POINT ( 'NONE',  ( 30.43807145043611584, -39.66766701456170097, 8.000000000000000000 ) ) ;
#11810 = CARTESIAN_POINT ( 'NONE',  ( -37.12029293941441210, -89.61631465359452875, 8.000000000000000000 ) ) ;
#11811 = VECTOR ( 'NONE', #9085, 1000.000000000000227 ) ;
#11812 = ORIENTED_EDGE ( 'NONE', *, *, #9362, .F. ) ;
#11813 = CIRCLE ( 'NONE', #904, 50.00000000000000000 ) ;
#11814 = CYLINDRICAL_SURFACE ( 'NONE', #3795, 59.50000000000000000 ) ;
#11815 = CARTESIAN_POINT ( 'NONE',  ( 0.000000000000000000, 0.000000000000000000, -10.50000000000000000 ) ) ;
#11816 = DIRECTION ( 'NONE',  ( 1.000000000000000000, -4.440892098500626162E-15, 0.000000000000000000 ) ) ;
#11817 = VERTEX_POINT ( 'NONE', #9999 ) ;
#11818 = ORIENTED_EDGE ( 'NONE', *, *, #12369, .F. ) ;
#11819 = EDGE_LOOP ( 'NONE', ( #5982, #3484, #2954, #12530 ) ) ;
#11820 = CARTESIAN_POINT ( 'NONE',  ( -45.89934640057513349, 26.50000000000019540, -13.00000000000000178 ) ) ;
#11821 = CARTESIAN_POINT ( 'NONE',  ( 68.58935777509523746, 68.58935777509499587, -8.000000000000000000 ) ) ;
#11822 = DIRECTION ( 'NONE',  ( 1.000000000000000000, 0.000000000000000000, 0.000000000000000000 ) ) ;
#11823 = DIRECTION ( 'NONE',  ( 0.000000000000000000, 0.000000000000000000, 1.000000000000000000 ) ) ;
#11824 = ADVANCED_FACE ( 'NONE', ( #1953 ), #13496, .F. ) ;
#11825 = VERTEX_POINT ( 'NONE', #4394 ) ;
#11826 = EDGE_CURVE ( 'NONE', #5585, #9114, #2770, .T. ) ;
#11827 = EDGE_CURVE ( 'NONE', #12492, #1887, #10525, .T. ) ;
#11828 = ORIENTED_EDGE ( 'NONE', *, *, #9700, .T. ) ;
#11829 = EDGE_CURVE ( 'NONE', #7998, #13011, #5912, .T. ) ;
#11830 = DIRECTION ( 'NONE',  ( 0.000000000000000000, 0.000000000000000000, 1.000000000000000000 ) ) ;
#11831 = LINE ( 'NONE', #3707, #934 ) ;
#11832 = LINE ( 'NONE', #14321, #12458 ) ;
#11833 = ADVANCED_FACE ( 'NONE', ( #9005 ), #13647, .F. ) ;
#11834 = VERTEX_POINT ( 'NONE', #673 ) ;
#11835 = ORIENTED_EDGE ( 'NONE', *, *, #12941, .T. ) ;
#11836 = ORIENTED_EDGE ( 'NONE', *, *, #5512, .F. ) ;
#11837 = DIRECTION ( 'NONE',  ( -1.000000000000000000, 0.000000000000000000, 0.000000000000000000 ) ) ;
#11838 = VERTEX_POINT ( 'NONE', #6719 ) ;
#11839 = CARTESIAN_POINT ( 'NONE',  ( 0.000000000000000000, 0.000000000000000000, -45.50000000000000000 ) ) ;
#11840 = LINE ( 'NONE', #6397, #533 ) ;
#11841 = CARTESIAN_POINT ( 'NONE',  ( 6.917888187663118416, 52.54657765281190507, -8.000000000000000000 ) ) ;
#11842 = ADVANCED_FACE ( 'NONE', ( #13561 ), #6570, .F. ) ;
#11843 = DIRECTION ( 'NONE',  ( -0.000000000000000000, -0.000000000000000000, 1.000000000000000000 ) ) ;
#11844 = CARTESIAN_POINT ( 'NONE',  ( -10.20278626552728873, 74.30320229487229255, -19.21617406370430103 ) ) ;
#11845 = CIRCLE ( 'NONE', #13786, 3.000000000000002665 ) ;
#11846 = CARTESIAN_POINT ( 'NONE',  ( 25.00000000000000000, 81.24038404635960831, -26.00000000000000000 ) ) ;
#11847 = VERTEX_POINT ( 'NONE', #8698 ) ;
#11848 = ADVANCED_FACE ( 'NONE', ( #1808 ), #3173, .T. ) ;
#11849 = FACE_OUTER_BOUND ( 'NONE', #10887, .T. ) ;
#11850 = ORIENTED_EDGE ( 'NONE', *, *, #9865, .T. ) ;
#11851 = ORIENTED_EDGE ( 'NONE', *, *, #10063, .T. ) ;
#11852 = CARTESIAN_POINT ( 'NONE',  ( 3.999999999999996447, -1.560351142792951951, -0.2242961665059788889 ) ) ;
#11853 = CARTESIAN_POINT ( 'NONE',  ( -30.00000000000000711, 97.48846085563154418, 31.00000000000000000 ) ) ;
#11854 = DIRECTION ( 'NONE',  ( 0.000000000000000000, 0.000000000000000000, -1.000000000000000000 ) ) ;
#11855 = CARTESIAN_POINT ( 'NONE',  ( 0.000000000000000000, 0.000000000000000000, 26.00000000000000000 ) ) ;
#11856 = CARTESIAN_POINT ( 'NONE',  ( -89.61631465359519666, -37.12029293941281338, -13.00000000000000178 ) ) ;
#11857 = DIRECTION ( 'NONE',  ( 0.000000000000000000, 0.000000000000000000, -1.000000000000000000 ) ) ;
#11858 = DIRECTION ( 'NONE',  ( -0.000000000000000000, -0.000000000000000000, -1.000000000000000000 ) ) ;
#11859 = CONTEXT_DEPENDENT_SHAPE_REPRESENTATION ( #13199, #9974 ) ;
#11860 = ORIENTED_EDGE ( 'NONE', *, *, #14225, .F. ) ;
#11861 = DIRECTION ( 'NONE',  ( 0.000000000000000000, 0.000000000000000000, 1.000000000000000000 ) ) ;
#11862 = ORIENTED_EDGE ( 'NONE', *, *, #14457, .T. ) ;
#11863 = CARTESIAN_POINT ( 'NONE',  ( -12.50000000000000000, 106.2673515243511133, -15.33083626825422918 ) ) ;
#11864 = AXIS2_PLACEMENT_3D ( 'NONE', #7732, #12310, #8719 ) ;
#11865 = LINE ( 'NONE', #11949, #1057 ) ;
#11866 = EDGE_CURVE ( 'NONE', #13570, #10850, #4247, .T. ) ;
#11867 = EDGE_CURVE ( 'NONE', #8628, #14193, #8860, .T. ) ;
#11868 = CARTESIAN_POINT ( 'NONE',  ( 68.68541276968825571, -69.08004447556089644, 10.49999999999999822 ) ) ;
#11869 = CARTESIAN_POINT ( 'NONE',  ( 2.500000000000002220, 2.357898499370430834, -6.938893903907228378E-15 ) ) ;
#11870 = ORIENTED_EDGE ( 'NONE', *, *, #10007, .T. ) ;
#11871 = CARTESIAN_POINT ( 'NONE',  ( 4.197393957002299558, -0.4069871074557456780, -3.503767560748925813 ) ) ;
#11872 = MECHANICAL_DESIGN_GEOMETRIC_PRESENTATION_REPRESENTATION (  '', ( #2405 ), #15026 ) ;
#11873 = VERTEX_POINT ( 'NONE', #10078 ) ;
#11874 = FACE_OUTER_BOUND ( 'NONE', #1127, .T. ) ;
#11875 = FACE_OUTER_BOUND ( 'NONE', #5360, .T. ) ;
#11876 = EDGE_CURVE ( 'NONE', #1886, #5824, #4212, .T. ) ;
#11877 = CIRCLE ( 'NONE', #2409, 2.649999999999987477 ) ;
#11878 = CARTESIAN_POINT ( 'NONE',  ( -35.79345569434273244, 100.4135791079098112, -16.00000000000000355 ) ) ;
#11879 = DIRECTION ( 'NONE',  ( 1.000000000000000000, 0.000000000000000000, 0.000000000000000000 ) ) ;
#11880 = B_SPLINE_CURVE_WITH_KNOTS ( 'NONE', 3,
 ( #12168, #1763, #631, #5256, #14517, #4115, #6746, #10336 ),
 .UNSPECIFIED., .F., .F.,
 ( 4, 2, 2, 4 ),
 ( 0.005725059856848646080, 0.006314084072593634418, 0.006903108288338622757, 0.008081156719828598567 ),
 .UNSPECIFIED. ) ;
#11881 = ORIENTED_EDGE ( 'NONE', *, *, #3367, .F. ) ;
#11882 = VERTEX_POINT ( 'NONE', #14723 ) ;
#11883 = FACE_OUTER_BOUND ( 'NONE', #5232, .T. ) ;
#11884 = CARTESIAN_POINT ( 'NONE',  ( 2.449293598294700991E-16, -97.00000000000000000, 8.000000000000000000 ) ) ;
#11885 = VECTOR ( 'NONE', #14227, 1000.000000000000000 ) ;
#11886 = EDGE_CURVE ( 'NONE', #6680, #3464, #5651, .T. ) ;
#11887 = CARTESIAN_POINT ( 'NONE',  ( 66.70695371924546180, 57.06275842387054098, -8.000000000000000000 ) ) ;
#11888 = CIRCLE ( 'NONE', #8239, 59.50000000000000711 ) ;
#11889 = CIRCLE ( 'NONE', #735, 0.5000000000000004441 ) ;
#11890 = AXIS2_PLACEMENT_3D ( 'NONE', #7131, #10711, #3657 ) ;
#11891 = ORIENTED_EDGE ( 'NONE', *, *, #5175, .F. ) ;
#11892 = ORIENTED_EDGE ( 'NONE', *, *, #3818, .T. ) ;
#11893 = FACE_OUTER_BOUND ( 'NONE', #9986, .T. ) ;
#11894 = CARTESIAN_POINT ( 'NONE',  ( 0.000000000000000000, -4.618802153517023612, -3.433295621305388678 ) ) ;
#11895 = AXIS2_PLACEMENT_3D ( 'NONE', #9953, #3063, #3282 ) ;
#11896 = CARTESIAN_POINT ( 'NONE',  ( -7.383907457637922889, -52.72775723226778410, -10.50000000000000000 ) ) ;
#11897 = CARTESIAN_POINT ( 'NONE',  ( 14.70911110638339814, -51.49712671369398720, -10.50000000000000000 ) ) ;
#11898 =( NAMED_UNIT ( * ) SI_UNIT ( $, .STERADIAN. ) SOLID_ANGLE_UNIT ( ) );
#11899 = DIRECTION ( 'NONE',  ( 0.000000000000000000, 0.000000000000000000, 1.000000000000000000 ) ) ;
#11900 = VECTOR ( 'NONE', #312, 1000.000000000000000 ) ;
#11901 = ORIENTED_EDGE ( 'NONE', *, *, #12247, .F. ) ;
#11902 = B_SPLINE_CURVE_WITH_KNOTS ( 'NONE', 3,
 ( #10137, #3316, #736, #10292, #6559, #14858, #4533, #3164, #8997, #3091, #7785, #2098, #9149, #4236, #6636, #7636, #12505, #12284, #6711, #13720 ),
 .UNSPECIFIED., .F., .F.,
 ( 4, 2, 2, 2, 2, 2, 2, 2, 2, 4 ),
 ( 0.000000000000000000, 0.0009816351435713618467, 0.001472452715357043746, 0.001963270287142725428, 0.002944905430714073180, 0.003926540574285420498, 0.004908175717856767817, 0.005889810861428116003, 0.006871446004999463321, 0.007853081148570811507 ),
 .UNSPECIFIED. ) ;
#11903 = ORIENTED_EDGE ( 'NONE', *, *, #9716, .F. ) ;
#11904 = VECTOR ( 'NONE', #7258, 1000.000000000000000 ) ;
#11905 = EDGE_LOOP ( 'NONE', ( #7490, #6485, #11201, #4476 ) ) ;
#11906 = EDGE_LOOP ( 'NONE', ( #4689, #8182, #1645, #3969, #12193, #4048 ) ) ;
#11907 = DIRECTION ( 'NONE',  ( 0.000000000000000000, 0.000000000000000000, 1.000000000000000000 ) ) ;
#11908 = DIRECTION ( 'NONE',  ( 0.000000000000000000, 0.000000000000000000, -1.000000000000000000 ) ) ;
#11909 = CARTESIAN_POINT ( 'NONE',  ( -2.499999999999999556, 3.061616997868382648E-16, 3.469446951953614189E-15 ) ) ;
#11910 = ORIENTED_EDGE ( 'NONE', *, *, #5136, .T. ) ;
#11911 = AXIS2_PLACEMENT_3D ( 'NONE', #8435, #11861, #10792 ) ;
#11912 = AXIS2_PLACEMENT_3D ( 'NONE', #10156, #5468, #4261 ) ;
#11913 = ORIENTED_EDGE ( 'NONE', *, *, #451, .F. ) ;
#11914 = CARTESIAN_POINT ( 'NONE',  ( -32.06294366074467206, 42.50536573064442081, -10.50000000000000000 ) ) ;
#11915 = AXIS2_PLACEMENT_3D ( 'NONE', #390, #7206, #10931 ) ;
#11916 = ORIENTED_EDGE ( 'NONE', *, *, #11094, .F. ) ;
#11917 = AXIS2_PLACEMENT_3D ( 'NONE', #14466, #9594, #652 ) ;
#11918 = EDGE_CURVE ( 'NONE', #14678, #6775, #12209, .T. ) ;
#11919 = DIRECTION ( 'NONE',  ( -1.000000000000000000, 0.000000000000000000, 0.000000000000000000 ) ) ;
#11920 = EDGE_CURVE ( 'NONE', #12353, #5584, #12928, .T. ) ;
#11921 = DIRECTION ( 'NONE',  ( -1.000000000000000000, 0.000000000000000000, 0.000000000000000000 ) ) ;
#11923 = AXIS2_PLACEMENT_3D ( 'NONE', #3398, #8023, #2110 ) ;
#11922 = DIRECTION ( 'NONE',  ( 0.000000000000000000, 0.000000000000000000, 1.000000000000000000 ) ) ;
#11924 = DIRECTION ( 'NONE',  ( 0.000000000000000000, 0.000000000000000000, 1.000000000000000000 ) ) ;
#11925 = ORIENTED_EDGE ( 'NONE', *, *, #1460, .F. ) ;
#11926 = AXIS2_PLACEMENT_3D ( 'NONE', #2029, #6647, #4392 ) ;
#11927 = CARTESIAN_POINT ( 'NONE',  ( -33.48561063518626923, 47.21331623427104063, 8.000000000000000000 ) ) ;
#11928 = AXIS2_PLACEMENT_3D ( 'NONE', #1244, #1400, #11728 ) ;
#11929 = ORIENTED_EDGE ( 'NONE', *, *, #8325, .T. ) ;
#11930 = ORIENTED_EDGE ( 'NONE', *, *, #3605, .F. ) ;
#11931 = PRODUCT_RELATED_PRODUCT_CATEGORY ( 'part', '', ( #12162 ) ) ;
#11932 = DIRECTION ( 'NONE',  ( -1.000000000000000000, 0.000000000000000000, 0.000000000000000000 ) ) ;
#11933 = CIRCLE ( 'NONE', #6089, 3.000000000000002665 ) ;
#11934 = FACE_OUTER_BOUND ( 'NONE', #12907, .T. ) ;
#11935 = ORIENTED_EDGE ( 'NONE', *, *, #13230, .T. ) ;
#11936 = ADVANCED_FACE ( 'NONE', ( #4543 ), #7941, .F. ) ;
#11937 = EDGE_CURVE ( 'NONE', #14224, #9901, #11489, .T. ) ;
#11938 = DIRECTION ( 'NONE',  ( 0.000000000000000000, 0.000000000000000000, -1.000000000000000000 ) ) ;
#11939 = AXIS2_PLACEMENT_3D ( 'NONE', #2410, #1712, #6318 ) ;
#11940 = DIRECTION ( 'NONE',  ( 0.000000000000000000, 0.000000000000000000, 1.000000000000000000 ) ) ;
#11941 = DIRECTION ( 'NONE',  ( 1.000000000000000000, 0.000000000000000000, 0.000000000000000000 ) ) ;
#11942 = CARTESIAN_POINT ( 'NONE',  ( 0.6507732100473456738, -4.243078065514790609, -0.2236248678334918361 ) ) ;
#11943 = CARTESIAN_POINT ( 'NONE',  ( -2.000000000000008882, -3.464101615137750390, 0.000000000000000000 ) ) ;
#11944 = ORIENTED_EDGE ( 'NONE', *, *, #11370, .T. ) ;
#11945 = APPLICATION_CONTEXT ( 'automotive_design' ) ;
#11946 = DIRECTION ( 'NONE',  ( 0.000000000000000000, 0.000000000000000000, 1.000000000000000000 ) ) ;
#11947 = ORIENTED_EDGE ( 'NONE', *, *, #694, .T. ) ;
#11948 = CARTESIAN_POINT ( 'NONE',  ( -12.50000000000000000, 106.2673515243510991, -15.00000000000000000 ) ) ;
#11949 = CARTESIAN_POINT ( 'NONE',  ( 29.70588235294119173, 96.53269163155674448, -10.99999999999999645 ) ) ;
#11950 = CIRCLE ( 'NONE', #10481, 0.5000000000000004441 ) ;
#11951 = CARTESIAN_POINT ( 'NONE',  ( 0.000000000000000000, 0.000000000000000000, 8.000000000000000000 ) ) ;
#11952 = CARTESIAN_POINT ( 'NONE',  ( -50.00000000000000000, 0.000000000000000000, -13.00000000000000178 ) ) ;
#11953 = ORIENTED_EDGE ( 'NONE', *, *, #1585, .T. ) ;
#11954 = CARTESIAN_POINT ( 'NONE',  ( 4.197393957002300446, 7.760817478283647932E-14, -3.503767560748928922 ) ) ;
#11955 = VERTEX_POINT ( 'NONE', #970 ) ;
#11956 = AXIS2_PLACEMENT_3D ( 'NONE', #8532, #187, #13175 ) ;
#11957 = CARTESIAN_POINT ( 'NONE',  ( 0.000000000000000000, 0.000000000000000000, -4.974599999999998801 ) ) ;
#11958 = CARTESIAN_POINT ( 'NONE',  ( 44.89637028918152595, -6.028507236160502272E-15, -25.50000000000000355 ) ) ;
#11959 = DIRECTION ( 'NONE',  ( 1.000000000000000000, 0.000000000000000000, 0.000000000000000000 ) ) ;
#11960 = EDGE_CURVE ( 'NONE', #8252, #14878, #6353, .T. ) ;
#11961 = CIRCLE ( 'NONE', #10912, 50.00000000000000000 ) ;
#11962 = LINE ( 'NONE', #6167, #10037 ) ;
#11963 = EDGE_CURVE ( 'NONE', #6056, #7966, #7820, .T. ) ;
#11964 = ORIENTED_EDGE ( 'NONE', *, *, #1474, .T. ) ;
#11965 = DIRECTION ( 'NONE',  ( 1.000000000000000000, 0.000000000000000000, 0.000000000000000000 ) ) ;
#11966 = DIRECTION ( 'NONE',  ( 0.000000000000000000, 0.000000000000000000, 1.000000000000000000 ) ) ;
#11967 = AXIS2_PLACEMENT_3D ( 'NONE', #9279, #19, #4581 ) ;
#11968 = DIRECTION ( 'NONE',  ( -1.000000000000000000, 0.000000000000000000, 0.000000000000000000 ) ) ;
#11969 = EDGE_CURVE ( 'NONE', #7984, #143, #12660, .T. ) ;
#11970 = AXIS2_PLACEMENT_3D ( 'NONE', #4517, #11584, #1170 ) ;
#11971 = ORIENTED_EDGE ( 'NONE', *, *, #8463, .T. ) ;
#11972 = CARTESIAN_POINT ( 'NONE',  ( 0.000000000000000000, 0.000000000000000000, -25.50000000000000355 ) ) ;
#11973 = VECTOR ( 'NONE', #193, 1000.000000000000000 ) ;
#11974 = ORIENTED_EDGE ( 'NONE', *, *, #10614, .F. ) ;
#11975 = CARTESIAN_POINT ( 'NONE',  ( -37.12029293941441210, -89.61631465359452875, -13.00000000000000178 ) ) ;
#11976 = VERTEX_POINT ( 'NONE', #8170 ) ;
#11977 = EDGE_CURVE ( 'NONE', #13764, #6523, #10495, .T. ) ;
#11978 = AXIS2_PLACEMENT_3D ( 'NONE', #287, #9836, #8470 ) ;
#11979 = CARTESIAN_POINT ( 'NONE',  ( 0.000000000000000000, 0.000000000000000000, -10.50000000000000000 ) ) ;
#11980 = EDGE_CURVE ( 'NONE', #8921, #9550, #3955, .T. ) ;
#11981 = CARTESIAN_POINT ( 'NONE',  ( 2.500000000000002220, 2.357898499370430834, -6.938893903907228378E-15 ) ) ;
#11982 =( LENGTH_UNIT ( ) NAMED_UNIT ( * ) SI_UNIT ( .MILLI., .METRE. ) );
#11983 = CARTESIAN_POINT ( 'NONE',  ( -33.83031011230892915, 95.16624652083667968, -15.96768307234233397 ) ) ;
#11984 = VERTEX_POINT ( 'NONE', #11679 ) ;
#11985 = ORIENTED_EDGE ( 'NONE', *, *, #13646, .F. ) ;
#11986 = ORIENTED_EDGE ( 'NONE', *, *, #1529, .T. ) ;
#11987 = CARTESIAN_POINT ( 'NONE',  ( 51.53979475227119167, 13.35619814848851483, -10.50000000000000000 ) ) ;
#11988 = CARTESIAN_POINT ( 'NONE',  ( -42.04772703543551415, -32.26435573746212526, -8.000000000000000000 ) ) ;
#11989 = CIRCLE ( 'NONE', #10996, 0.5000000000000022204 ) ;
#11990 = LINE ( 'NONE', #12059, #10263 ) ;
#11991 = VERTEX_POINT ( 'NONE', #2256 ) ;
#11992 = ORIENTED_EDGE ( 'NONE', *, *, #7066, .F. ) ;
#11993 = PLANE ( 'NONE',  #8117 ) ;
#11994 = VERTEX_POINT ( 'NONE', #13883 ) ;
#11995 = CIRCLE ( 'NONE', #12950, 53.55662432702593634 ) ;
#11997 = CARTESIAN_POINT ( 'NONE',  ( 2.649999999999987033, 38.00000000000000000, -25.50000000000000355 ) ) ;
#11996 = AXIS2_PLACEMENT_3D ( 'NONE', #8339, #1733, #3941 ) ;
#11998 = CIRCLE ( 'NONE', #2045, 50.00000000000000000 ) ;
#11999 = CARTESIAN_POINT ( 'NONE',  ( 2.807080416178797666, -3.225969019225332524, -3.502507215260528994 ) ) ;
#12000 = DIRECTION ( 'NONE',  ( -0.000000000000000000, -0.000000000000000000, 1.000000000000000000 ) ) ;
#12001 = ORIENTED_EDGE ( 'NONE', *, *, #3098, .T. ) ;
#12002 = CARTESIAN_POINT ( 'NONE',  ( 6.451868917687939131, 52.36539807335604024, 10.49999999999999822 ) ) ;
#12003 = DIRECTION ( 'NONE',  ( 0.000000000000000000, 0.000000000000000000, -1.000000000000000000 ) ) ;
#12004 = ORIENTED_EDGE ( 'NONE', *, *, #10261, .F. ) ;
#12005 = CARTESIAN_POINT ( 'NONE',  ( -100.0000000000000000, 0.000000000000000000, -13.00000000000000178 ) ) ;
#12006 = AXIS2_PLACEMENT_3D ( 'NONE', #8468, #9905, #5216 ) ;
#12007 = ORIENTED_EDGE ( 'NONE', *, *, #12524, .T. ) ;
#12008 = CIRCLE ( 'NONE', #14909, 2.499999999999999556 ) ;
#12009 = EDGE_LOOP ( 'NONE', ( #1361, #6919, #12391, #7486 ) ) ;
#12010 = DIRECTION ( 'NONE',  ( 0.000000000000000000, 0.000000000000000000, 1.000000000000000000 ) ) ;
#12011 = DIRECTION ( 'NONE',  ( 1.000000000000000000, 0.000000000000000000, -0.000000000000000000 ) ) ;
#12012 = AXIS2_PLACEMENT_3D ( 'NONE', #9605, #6326, #9749 ) ;
#12013 = DIRECTION ( 'NONE',  ( 1.000000000000000000, 0.000000000000000000, 0.000000000000000000 ) ) ;
#12014 = CARTESIAN_POINT ( 'NONE',  ( 94.51066581171355097, 1.674280531758986834, -13.00000000000000178 ) ) ;
#12015 = DIRECTION ( 'NONE',  ( -1.000000000000000000, 0.000000000000000000, 0.000000000000000000 ) ) ;
#12016 = CIRCLE ( 'NONE', #11030, 0.5000000000000073275 ) ;
#12017 = CIRCLE ( 'NONE', #369, 102.0000000000000142 ) ;
#12018 = DIRECTION ( 'NONE',  ( 1.000000000000000000, 0.000000000000000000, 0.000000000000000000 ) ) ;
#12019 = ORIENTED_EDGE ( 'NONE', *, *, #4218, .T. ) ;
#12020 = DIRECTION ( 'NONE',  ( 0.000000000000000000, 0.000000000000000000, -1.000000000000000000 ) ) ;
#12021 = ORIENTED_EDGE ( 'NONE', *, *, #4887, .T. ) ;
#12022 = ADVANCED_FACE ( 'NONE', ( #6871 ), #12880, .F. ) ;
#12023 = EDGE_CURVE ( 'NONE', #10391, #215, #14143, .T. ) ;
#12024 = ADVANCED_FACE ( 'NONE', ( #11539, #48 ), #8090, .T. ) ;
#12025 = CARTESIAN_POINT ( 'NONE',  ( 49.00442420935993226, -30.80502811811213704, -8.000000000000000000 ) ) ;
#12026 = CARTESIAN_POINT ( 'NONE',  ( -3.999999999999996447, 2.309401076758498039, -5.000000000000000888 ) ) ;
#12027 = MECHANICAL_DESIGN_GEOMETRIC_PRESENTATION_REPRESENTATION (  '', ( #117 ), #13709 ) ;
#12028 = CARTESIAN_POINT ( 'NONE',  ( 12.86891638962116247, -56.43380494354001087, -10.50000000000000000 ) ) ;
#12029 = CIRCLE ( 'NONE', #8611, 50.00000000000000000 ) ;
#12030 = DIRECTION ( 'NONE',  ( 0.000000000000000000, 0.000000000000000000, 1.000000000000000000 ) ) ;
#12031 = ORIENTED_EDGE ( 'NONE', *, *, #12616, .T. ) ;
#12032 = DIRECTION ( 'NONE',  ( -0.000000000000000000, -0.000000000000000000, -1.000000000000000000 ) ) ;
#12033 = ORIENTED_EDGE ( 'NONE', *, *, #6929, .T. ) ;
#12034 = ORIENTED_EDGE ( 'NONE', *, *, #42, .F. ) ;
#12035 = CARTESIAN_POINT ( 'NONE',  ( -14.70911110638303754, 51.49712671369408667, -10.50000000000000000 ) ) ;
#12036 = DIRECTION ( 'NONE',  ( 1.000000000000000000, 8.746504920891464822E-16, 0.000000000000000000 ) ) ;
#12037 = AXIS2_PLACEMENT_3D ( 'NONE', #582, #5285, #5215 ) ;
#12038 = AXIS2_PLACEMENT_3D ( 'NONE', #14801, #11385, #3406 ) ;
#12039 = DIRECTION ( 'NONE',  ( -1.000000000000000000, 0.000000000000000000, 0.000000000000000000 ) ) ;
#12040 = CYLINDRICAL_SURFACE ( 'NONE', #10505, 59.50000000000000000 ) ;
#12041 = DIRECTION ( 'NONE',  ( -1.000000000000000000, 0.000000000000000000, 0.000000000000000000 ) ) ;
#12042 = VERTEX_POINT ( 'NONE', #11454 ) ;
#12043 = DIRECTION ( 'NONE',  ( 1.000000000000000000, 0.000000000000000000, 0.000000000000000000 ) ) ;
#12044 = DIRECTION ( 'NONE',  ( 0.000000000000000000, 0.000000000000000000, 1.000000000000000000 ) ) ;
#12045 = CARTESIAN_POINT ( 'NONE',  ( 55.00000000000000711, 0.000000000000000000, 0.000000000000000000 ) ) ;
#12046 = CIRCLE ( 'NONE', #1845, 0.5000000000000004441 ) ;
#12047 = EDGE_CURVE ( 'NONE', #14464, #11082, #2987, .T. ) ;
#12048 = EDGE_LOOP ( 'NONE', ( #11903, #8010, #9451, #2347 ) ) ;
#12049 = DIRECTION ( 'NONE',  ( 0.000000000000000000, 0.000000000000000000, 1.000000000000000000 ) ) ;
#12050 = VERTEX_POINT ( 'NONE', #12739 ) ;
#12051 = LINE ( 'NONE', #7541, #9796 ) ;
#12052 = VERTEX_POINT ( 'NONE', #10447 ) ;
#12053 = DIRECTION ( 'NONE',  ( 1.000000000000000000, 0.000000000000000000, -0.000000000000000000 ) ) ;
#12054 = CARTESIAN_POINT ( 'NONE',  ( 24.98583958711424202, -30.74264578624780597, -25.50000000000000355 ) ) ;
#12055 = LINE ( 'NONE', #10826, #2082 ) ;
#12056 = ORIENTED_EDGE ( 'NONE', *, *, #6715, .F. ) ;
#12057 = CYLINDRICAL_SURFACE ( 'NONE', #7629, 2.649999999999985700 ) ;
#12058 = DIRECTION ( 'NONE',  ( 1.000000000000000000, 0.000000000000000000, 0.000000000000000000 ) ) ;
#12059 = CARTESIAN_POINT ( 'NONE',  ( 12.50000000000000000, 106.2673515243510991, -31.00000000000000000 ) ) ;
#12060 = ORIENTED_EDGE ( 'NONE', *, *, #7670, .T. ) ;
#12061 = ADVANCED_FACE ( 'NONE', ( #2330 ), #2868, .F. ) ;
#12062 = EDGE_CURVE ( 'NONE', #13092, #14329, #9598, .T. ) ;
#12063 = EDGE_LOOP ( 'NONE', ( #5202, #8403, #8434, #12829, #8535, #1363 ) ) ;
#12064 = DIRECTION ( 'NONE',  ( -0.000000000000000000, -0.000000000000000000, 1.000000000000000000 ) ) ;
#12065 = ORIENTED_EDGE ( 'NONE', *, *, #3434, .F. ) ;
#12066 = CARTESIAN_POINT ( 'NONE',  ( -37.71449950290985953, 86.67575032682117353, -8.000000000000000000 ) ) ;
#12067 = CARTESIAN_POINT ( 'NONE',  ( 3.455068668934434317, -2.624017327439083669, -3.316620875263605051 ) ) ;
#12068 = ADVANCED_FACE ( 'NONE', ( #9524 ), #13261, .F. ) ;
#12069 = LINE ( 'NONE', #1660, #1241 ) ;
#12070 = CARTESIAN_POINT ( 'NONE',  ( -3.492805317593278058, 46.55633131742322917, -10.50000000000000000 ) ) ;
#12071 = ORIENTED_EDGE ( 'NONE', *, *, #2597, .F. ) ;
#12072 = DIRECTION ( 'NONE',  ( 0.000000000000000000, 0.000000000000000000, 1.000000000000000000 ) ) ;
#12073 = VECTOR ( 'NONE', #13292, 1000.000000000000000 ) ;
#12074 = ORIENTED_EDGE ( 'NONE', *, *, #7814, .F. ) ;
#12075 = EDGE_CURVE ( 'NONE', #9694, #1381, #3925, .T. ) ;
#12076 = EDGE_LOOP ( 'NONE', ( #11796, #551, #8442, #12642 ) ) ;
#12077 = DIRECTION ( 'NONE',  ( 0.000000000000000000, 0.000000000000000000, -1.000000000000000000 ) ) ;
#12078 = ORIENTED_EDGE ( 'NONE', *, *, #11512, .T. ) ;
#12079 = CARTESIAN_POINT ( 'NONE',  ( 31.95756590787640050, 102.1116157579503181, -13.22695225398608088 ) ) ;
#12080 = CIRCLE ( 'NONE', #5531, 59.50000000000000000 ) ;
#12081 = CARTESIAN_POINT ( 'NONE',  ( 0.000000000000000000, 0.000000000000000000, -13.50000000000000178 ) ) ;
#12082 = CARTESIAN_POINT ( 'NONE',  ( 2.500000000000002220, 1.178949249685208533, -2.042000000000002036 ) ) ;
#12083 = DIRECTION ( 'NONE',  ( -1.000000000000000000, 0.000000000000000000, 0.000000000000000000 ) ) ;
#12084 = CARTESIAN_POINT ( 'NONE',  ( -24.98583958711379083, -30.74264578624812927, 14.49999999999999822 ) ) ;
#12085 = ORIENTED_EDGE ( 'NONE', *, *, #1001, .T. ) ;
#12086 = CYLINDRICAL_SURFACE ( 'NONE', #6784, 101.0000000000000284 ) ;
#12087 = B_SPLINE_CURVE_WITH_KNOTS ( 'NONE', 3,
 ( #5319, #4423, #2971, #13449 ),
 .UNSPECIFIED., .F., .F.,
 ( 4, 4 ),
 ( 0.000000000000000000, 0.002452478801916362864 ),
 .UNSPECIFIED. ) ;
#12088 = ORIENTED_EDGE ( 'NONE', *, *, #7731, .F. ) ;
#12089 = CARTESIAN_POINT ( 'NONE',  ( -51.53979475227126983, -13.35619814848815601, -10.50000000000000000 ) ) ;
#12090 = DIRECTION ( 'NONE',  ( -1.000000000000000000, 0.000000000000000000, 0.000000000000000000 ) ) ;
#12091 = ORIENTED_EDGE ( 'NONE', *, *, #9779, .F. ) ;
#12092 = DIRECTION ( 'NONE',  ( -0.000000000000000000, -0.000000000000000000, 1.000000000000000000 ) ) ;
#12093 = CARTESIAN_POINT ( 'NONE',  ( 3.999999999999996447, 2.309401076758498039, -5.000000000000000888 ) ) ;
#12094 = EDGE_LOOP ( 'NONE', ( #3160, #1637, #14559, #3234 ) ) ;
#12095 = PLANE ( 'NONE',  #2897 ) ;
#12096 = ORIENTED_EDGE ( 'NONE', *, *, #6698, .F. ) ;
#12097 = DIRECTION ( 'NONE',  ( -0.000000000000000000, -1.000000000000000000, -0.000000000000000000 ) ) ;
#12098 = EDGE_CURVE ( 'NONE', #11105, #13418, #5163, .T. ) ;
#12099 = CARTESIAN_POINT ( 'NONE',  ( 0.000000000000000000, 0.000000000000000000, 8.000000000000000000 ) ) ;
#12100 = ADVANCED_FACE ( 'NONE', ( #10892, #496, #3779, #8397, #6025, #8461, #10824 ), #9662, .F. ) ;
#12101 = CARTESIAN_POINT ( 'NONE',  ( -35.08068705722485703, 100.7955773171491813, -15.87635720896652103 ) ) ;
#12102 = DIRECTION ( 'NONE',  ( 0.000000000000000000, 0.000000000000000000, -1.000000000000000000 ) ) ;
#12103 = CARTESIAN_POINT ( 'NONE',  ( 68.49330278050122445, -68.09867107463004743, -10.50000000000000000 ) ) ;
#12104 = ORIENTED_EDGE ( 'NONE', *, *, #14880, .T. ) ;
#12105 = CARTESIAN_POINT ( 'NONE',  ( 9.718176292668216476, 74.36971601906103047, -19.51774219187060311 ) ) ;
#12106 = CARTESIAN_POINT ( 'NONE',  ( -47.21331623427138879, -33.48561063518577896, -13.00000000000000178 ) ) ;
#12107 = DIRECTION ( 'NONE',  ( 0.000000000000000000, 0.000000000000000000, 1.000000000000000000 ) ) ;
#12108 = UNCERTAINTY_MEASURE_WITH_UNIT (LENGTH_MEASURE( 1.000000000000000082E-05 ), #12583, 'distance_accuracy_value', 'NONE');
#12109 = ORIENTED_EDGE ( 'NONE', *, *, #6844, .T. ) ;
#12110 = CARTESIAN_POINT ( 'NONE',  ( 0.000000000000000000, -4.618802153517023612, -5.000000000000000888 ) ) ;
#12111 = CIRCLE ( 'NONE', #1681, 101.0000000000000284 ) ;
#12112 = ORIENTED_EDGE ( 'NONE', *, *, #8673, .F. ) ;
#12113 = DIRECTION ( 'NONE',  ( 1.000000000000000000, 0.000000000000000000, 0.000000000000000000 ) ) ;
#12114 = EDGE_CURVE ( 'NONE', #1055, #1207, #1778, .T. ) ;
#12115 = FACE_OUTER_BOUND ( 'NONE', #14255, .T. ) ;
#12116 = CARTESIAN_POINT ( 'NONE',  ( 9.703618315745391243, 62.24871376222710495, -19.49715125027359974 ) ) ;
#12117 = DIRECTION ( 'NONE',  ( -1.000000000000000000, 0.000000000000000000, -0.000000000000000000 ) ) ;
#12118 = CARTESIAN_POINT ( 'NONE',  ( 36.14014761921570340, 11.74264578624841171, -33.00000000000000000 ) ) ;
#12119 = LINE ( 'NONE', #7172, #7153 ) ;
#12120 = PRODUCT_DEFINITION_FORMATION_WITH_SPECIFIED_SOURCE ( 'ANY', '', #4170, .NOT_KNOWN. ) ;
#12121 = ORIENTED_EDGE ( 'NONE', *, *, #6369, .F. ) ;
#12122 = FACE_OUTER_BOUND ( 'NONE', #822, .T. ) ;
#12123 = CIRCLE ( 'NONE', #8951, 3.000000000000002665 ) ;
#12124 = CARTESIAN_POINT ( 'NONE',  ( 33.48561063518626923, -47.21331623427104063, -13.00000000000000178 ) ) ;
#12125 = AXIS2_PLACEMENT_3D ( 'NONE', #846, #13510, #1970 ) ;
#12126 = CARTESIAN_POINT ( 'NONE',  ( -37.12029293941441210, -89.61631465359452875, -8.000000000000000000 ) ) ;
#12127 = ORIENTED_EDGE ( 'NONE', *, *, #7723, .F. ) ;
#12128 = VERTEX_POINT ( 'NONE', #277 ) ;
#12129 = DIRECTION ( 'NONE',  ( 1.000000000000000000, 0.000000000000000000, -0.000000000000000000 ) ) ;
#12130 = CYLINDRICAL_SURFACE ( 'NONE', #13627, 10.00000000000000178 ) ;
#12131 = ORIENTED_EDGE ( 'NONE', *, *, #1376, .F. ) ;
#12132 = VECTOR ( 'NONE', #8422, 1000.000000000000000 ) ;
#12133 = AXIS2_PLACEMENT_3D ( 'NONE', #9804, #14296, #13305 ) ;
#12134 = DIRECTION ( 'NONE',  ( 1.000000000000000000, 0.000000000000000000, 0.000000000000000000 ) ) ;
#12135 = AXIS2_PLACEMENT_3D ( 'NONE', #2756, #9579, #2607 ) ;
#12136 = AXIS2_PLACEMENT_3D ( 'NONE', #12920, #1450, #1605 ) ;
#12137 = CARTESIAN_POINT ( 'NONE',  ( 2.712762565639232903, -3.052587955997690283, -3.430618716626819165 ) ) ;
#12138 = EDGE_CURVE ( 'NONE', #9656, #5604, #7085, .T. ) ;
#12139 = FACE_OUTER_BOUND ( 'NONE', #8064, .T. ) ;
#12140 = DIRECTION ( 'NONE',  ( -0.000000000000000000, -0.000000000000000000, -1.000000000000000000 ) ) ;
#12141 = EDGE_CURVE ( 'NONE', #6102, #13227, #1061, .T. ) ;
#12142 = ORIENTED_EDGE ( 'NONE', *, *, #10239, .F. ) ;
#12143 = CARTESIAN_POINT ( 'NONE',  ( -33.48561063518626923, 47.21331623427104063, -13.00000000000000178 ) ) ;
#12144 = TOROIDAL_SURFACE ( 'NONE', #5587, 5.384454397937118664, 0.5155456020628804703 ) ;
#12145 = VERTEX_POINT ( 'NONE', #4991 ) ;
#12146 = AXIS2_PLACEMENT_3D ( 'NONE', #6835, #9120, #1161 ) ;
#12147 = AXIS2_PLACEMENT_3D ( 'NONE', #4342, #13675, #5479 ) ;
#12148 = ORIENTED_EDGE ( 'NONE', *, *, #5612, .F. ) ;
#12149 = DIRECTION ( 'NONE',  ( 1.000000000000000000, 0.000000000000000000, 0.000000000000000000 ) ) ;
#12150 = EDGE_CURVE ( 'NONE', #10917, #10230, #1650, .T. ) ;
#12151 = CARTESIAN_POINT ( 'NONE',  ( -27.94117647058823550, 90.79807628710781842, -13.50000000000000178 ) ) ;
#12152 = CIRCLE ( 'NONE', #10203, 107.0000000000000284 ) ;
#12153 = CIRCLE ( 'NONE', #11176, 50.00000000000000000 ) ;
#12154 = DIRECTION ( 'NONE',  ( 0.000000000000000000, 0.000000000000000000, -1.000000000000000000 ) ) ;
#12155 = LINE ( 'NONE', #2255, #5835 ) ;
#12156 = FACE_OUTER_BOUND ( 'NONE', #8779, .T. ) ;
#12157 = CARTESIAN_POINT ( 'NONE',  ( -3.492805317593278058, 46.55633131742322917, -10.50000000000000000 ) ) ;
#12158 = EDGE_CURVE ( 'NONE', #11013, #1542, #6248, .T. ) ;
#12159 = AXIS2_PLACEMENT_3D ( 'NONE', #677, #6426, #5298 ) ;
#12160 = VERTEX_POINT ( 'NONE', #14393 ) ;
#12161 = CARTESIAN_POINT ( 'NONE',  ( -45.83364790889027773, 29.49928053175948506, -13.00000000000000178 ) ) ;
#12162 = PRODUCT ( 'BR-595', 'BR-595', '', ( #8616 ) ) ;
#12163 = CARTESIAN_POINT ( 'NONE',  ( -7.500000000000000888, 74.62405778299650194, 20.00000000000000000 ) ) ;
#12164 = CARTESIAN_POINT ( 'NONE',  ( -49.57224306869049713, 6.526309611002767852, 8.000000000000000000 ) ) ;
#12165 = DIRECTION ( 'NONE',  ( -1.000000000000000000, 0.000000000000000000, 0.000000000000000000 ) ) ;
#12166 = VERTEX_POINT ( 'NONE', #7237 ) ;
#12167 = CARTESIAN_POINT ( 'NONE',  ( 32.08430773043614437, 95.76884182151505343, -15.34120815717649222 ) ) ;
#12168 = CARTESIAN_POINT ( 'NONE',  ( 3.999999999999996447, 0.000000000000000000, 0.000000000000000000 ) ) ;
#12169 = ORIENTED_EDGE ( 'NONE', *, *, #7672, .T. ) ;
#12170 = DIRECTION ( 'NONE',  ( 0.000000000000000000, 0.000000000000000000, 1.000000000000000000 ) ) ;
#12171 = VERTEX_POINT ( 'NONE', #12054 ) ;
#12172 = DIRECTION ( 'NONE',  ( 0.000000000000000000, 0.000000000000000000, 1.000000000000000000 ) ) ;
#12173 = DIRECTION ( 'NONE',  ( -1.000000000000000000, 0.000000000000000000, 0.000000000000000000 ) ) ;
#12174 = DIRECTION ( 'NONE',  ( 0.000000000000000000, 0.000000000000000000, 1.000000000000000000 ) ) ;
#12175 = AXIS2_PLACEMENT_3D ( 'NONE', #3661, #8139, #8285 ) ;
#12176 = CARTESIAN_POINT ( 'NONE',  ( -36.08010649850015028, 100.2464683348682541, -16.00000000000000000 ) ) ;
#12177 = DIRECTION ( 'NONE',  ( 0.000000000000000000, 0.000000000000000000, -1.000000000000000000 ) ) ;
#12178 = CYLINDRICAL_SURFACE ( 'NONE', #1980, 60.50000000000000711 ) ;
#12179 = VERTEX_POINT ( 'NONE', #14095 ) ;
#12180 = AXIS2_PLACEMENT_3D ( 'NONE', #13402, #14771, #5277 ) ;
#12181 = DIRECTION ( 'NONE',  ( 0.000000000000000000, 0.000000000000000000, 1.000000000000000000 ) ) ;
#12182 = DIRECTION ( 'NONE',  ( 0.000000000000000000, 0.000000000000000000, 1.000000000000000000 ) ) ;
#12183 = UNCERTAINTY_MEASURE_WITH_UNIT (LENGTH_MEASURE( 1.000000000000000082E-05 ), #14644, 'distance_accuracy_value', 'NONE');
#12184 = FACE_OUTER_BOUND ( 'NONE', #10280, .T. ) ;
#12185 = EDGE_CURVE ( 'NONE', #7535, #7436, #10259, .T. ) ;
#12186 = ORIENTED_EDGE ( 'NONE', *, *, #13127, .T. ) ;
#12187 = SHAPE_REPRESENTATION ( 'BR-595', ( #3632, #9926, #9191, #3389, #9915, #7000, #231, #2652, #7734, #14289, #10164, #13084, #3379, #14059, #5313, #11637 ), #14785 ) ;
#12188 = DIRECTION ( 'NONE',  ( 1.000000000000000000, 0.000000000000000000, 0.000000000000000000 ) ) ;
#12189 = ORIENTED_EDGE ( 'NONE', *, *, #3480, .F. ) ;
#12190 = CIRCLE ( 'NONE', #309, 2.499999999999999556 ) ;
#12191 = CARTESIAN_POINT ( 'NONE',  ( 25.00000000000000000, 81.24038404635960831, 16.00000000000000000 ) ) ;
#12192 = CARTESIAN_POINT ( 'NONE',  ( -12.28339058173379783, 73.98737765342407613, 16.56626766863481137 ) ) ;
#12193 = ORIENTED_EDGE ( 'NONE', *, *, #8234, .T. ) ;
#12194 = CARTESIAN_POINT ( 'NONE',  ( -2.000000000000008882, -3.464101615137750390, 0.000000000000000000 ) ) ;
#12195 = CARTESIAN_POINT ( 'NONE',  ( 23.50071946824040836, 45.96504489226015977, -13.00000000000000178 ) ) ;
#12196 = DIRECTION ( 'NONE',  ( -1.000000000000000000, 0.000000000000000000, 6.123233995736766036E-17 ) ) ;
#12197 = VERTEX_POINT ( 'NONE', #11897 ) ;
#12198 = CIRCLE ( 'NONE', #7080, 52.50000000000000711 ) ;
#12199 = ORIENTED_EDGE ( 'NONE', *, *, #2303, .F. ) ;
#12200 = VECTOR ( 'NONE', #14461, 1000.000000000000000 ) ;
#12201 = CYLINDRICAL_SURFACE ( 'NONE', #3053, 63.00000000000000000 ) ;
#12202 = CARTESIAN_POINT ( 'NONE',  ( 0.000000000000000000, 0.000000000000000000, 8.000000000000000000 ) ) ;
#12203 = AXIS2_PLACEMENT_3D ( 'NONE', #10636, #9496, #324 ) ;
#12204 = ADVANCED_FACE ( 'NONE', ( #2555 ), #7170, .F. ) ;
#12205 = DIRECTION ( 'NONE',  ( -1.000000000000000000, 0.000000000000000000, 0.000000000000000000 ) ) ;
#12206 = EDGE_CURVE ( 'NONE', #1924, #6323, #2267, .T. ) ;
#12208 = ORIENTED_EDGE ( 'NONE', *, *, #14050, .F. ) ;
#12207 = EDGE_CURVE ( 'NONE', #1787, #13337, #8913, .T. ) ;
#12209 = CIRCLE ( 'NONE', #11721, 53.55662432702593634 ) ;
#12210 = EDGE_LOOP ( 'NONE', ( #8011, #15017, #14071, #14782 ) ) ;
#12211 = ORIENTED_EDGE ( 'NONE', *, *, #9033, .T. ) ;
#12212 = CARTESIAN_POINT ( 'NONE',  ( -25.00000000000000000, 81.24038404635962252, -26.00000000000000000 ) ) ;
#12213 = DIRECTION ( 'NONE',  ( -0.000000000000000000, -0.000000000000000000, -1.000000000000000000 ) ) ;
#12214 = ORIENTED_EDGE ( 'NONE', *, *, #13225, .F. ) ;
#12215 = AXIS2_PLACEMENT_3D ( 'NONE', #1715, #6320, #14705 ) ;
#12216 = PLANE ( 'NONE',  #12159 ) ;
#12217 = DIRECTION ( 'NONE',  ( -1.000000000000000000, 0.000000000000000000, 0.000000000000000000 ) ) ;
#12218 = EDGE_LOOP ( 'NONE', ( #5094, #9260, #381, #4134, #130, #7261 ) ) ;
#12219 = DIRECTION ( 'NONE',  ( -1.000000000000000000, 0.000000000000000000, 0.000000000000000000 ) ) ;
#12220 = ORIENTED_EDGE ( 'NONE', *, *, #8246, .F. ) ;
#12222 = ORIENTED_EDGE ( 'NONE', *, *, #2649, .F. ) ;
#12221 =( REPRESENTATION_RELATIONSHIP ('NONE','NONE', #12187, #12767 ) REPRESENTATION_RELATIONSHIP_WITH_TRANSFORMATION ( #1308 )SHAPE_REPRESENTATION_RELATIONSHIP( ) );
#12223 = CARTESIAN_POINT ( 'NONE',  ( -33.38013186279886924, 95.32466787866006541, 15.87266497586409919 ) ) ;
#12224 = CIRCLE ( 'NONE', #4234, 0.5000000000000004441 ) ;
#12225 = AXIS2_PLACEMENT_3D ( 'NONE', #3639, #1015, #9395 ) ;
#12226 = EDGE_CURVE ( 'NONE', #132, #9892, #9286, .T. ) ;
#12227 = DIRECTION ( 'NONE',  ( 1.000000000000000000, 0.000000000000000000, 0.000000000000000000 ) ) ;
#12228 = EDGE_CURVE ( 'NONE', #10230, #2995, #9898, .T. ) ;
#12229 = DIRECTION ( 'NONE',  ( 1.000000000000000000, 0.000000000000000000, 0.000000000000000000 ) ) ;
#12230 = DIRECTION ( 'NONE',  ( 1.000000000000000000, 0.000000000000000000, 0.000000000000000000 ) ) ;
#12231 = CARTESIAN_POINT ( 'NONE',  ( -2.649999999999994138, 38.00000000000000000, -28.00000000000000000 ) ) ;
#12232 = DIRECTION ( 'NONE',  ( -1.000000000000000000, 0.000000000000000000, 0.000000000000000000 ) ) ;
#12233 = ORIENTED_EDGE ( 'NONE', *, *, #1707, .F. ) ;
#12234 = CIRCLE ( 'NONE', #7614, 101.0000000000000284 ) ;
#12235 = AXIS2_PLACEMENT_3D ( 'NONE', #6059, #12996, #7124 ) ;
#12236 = VECTOR ( 'NONE', #15007, 1000.000000000000000 ) ;
#12237 = DIRECTION ( 'NONE',  ( 1.000000000000000000, 0.000000000000000000, 0.000000000000000000 ) ) ;
#12238 = AXIS2_PLACEMENT_3D ( 'NONE', #4318, #4389, #12134 ) ;
#12239 = DIRECTION ( 'NONE',  ( 1.000000000000000000, 0.000000000000000000, 0.000000000000000000 ) ) ;
#12240 = CARTESIAN_POINT ( 'NONE',  ( 51.19406879332056093, 13.71740939043382745, -8.000000000000000000 ) ) ;
#12241 = VERTEX_POINT ( 'NONE', #5208 ) ;
#12242 = SURFACE_STYLE_FILL_AREA ( #13296 ) ;
#12243 = ORIENTED_EDGE ( 'NONE', *, *, #9266, .T. ) ;
#12244 = ADVANCED_FACE ( 'NONE', ( #3002 ), #576, .T. ) ;
#12245 = CIRCLE ( 'NONE', #12968, 63.00000000000000000 ) ;
#12246 = FACE_BOUND ( 'NONE', #5029, .T. ) ;
#12247 = EDGE_CURVE ( 'NONE', #1887, #9608, #2748, .T. ) ;
#12248 = ORIENTED_EDGE ( 'NONE', *, *, #11523, .T. ) ;
#12249 = CIRCLE ( 'NONE', #13190, 107.0000000000000284 ) ;
#12250 = CIRCLE ( 'NONE', #11764, 3.000000000000002665 ) ;
#12251 = DIRECTION ( 'NONE',  ( 1.000000000000000000, 0.000000000000000000, -0.000000000000000000 ) ) ;
#12252 = AXIS2_PLACEMENT_3D ( 'NONE', #7497, #14501, #4033 ) ;
#12253 = ORIENTED_EDGE ( 'NONE', *, *, #4587, .F. ) ;
#12254 = CYLINDRICAL_SURFACE ( 'NONE', #1323, 3.000000000000002665 ) ;
#12255 = DIRECTION ( 'NONE',  ( 0.000000000000000000, 0.000000000000000000, 1.000000000000000000 ) ) ;
#12256 = DIRECTION ( 'NONE',  ( 0.000000000000000000, 0.000000000000000000, 1.000000000000000000 ) ) ;
#12257 = CARTESIAN_POINT ( 'NONE',  ( 65.64523757230274725, 68.01302780753375998, 8.000000000000000000 ) ) ;
#12258 = DIRECTION ( 'NONE',  ( 0.000000000000000000, 0.000000000000000000, 1.000000000000000000 ) ) ;
#12259 = EDGE_CURVE ( 'NONE', #13104, #4116, #4305, .T. ) ;
#12260 = ORIENTED_EDGE ( 'NONE', *, *, #10659, .T. ) ;
#12261 = CARTESIAN_POINT ( 'NONE',  ( -4.211140560182194292, 2.431303136016534250, -3.745885042887433958 ) ) ;
#12262 = COLOUR_RGB ( '', 0.09019608, 0.27058824, 0.51372549) ;
#12263 = VERTEX_POINT ( 'NONE', #14474 ) ;
#12264 = CARTESIAN_POINT ( 'NONE',  ( 91.27544013909738396, -39.61975340586587890, 8.000000000000000000 ) ) ;
#12265 = DIRECTION ( 'NONE',  ( 1.000000000000000000, 0.000000000000000000, 0.000000000000000000 ) ) ;
#12266 = CIRCLE ( 'NONE', #10560, 3.000000000000002665 ) ;
#12267 = LINE ( 'NONE', #5425, #10737 ) ;
#12268 = EDGE_CURVE ( 'NONE', #11078, #8551, #8548, .T. ) ;
#12269 = EDGE_LOOP ( 'NONE', ( #11350, #5388, #8640, #11682, #2630 ) ) ;
#12270 = CARTESIAN_POINT ( 'NONE',  ( -3.453038570459854739, -2.625189405340492055, -3.535263753545665022 ) ) ;
#12271 = VECTOR ( 'NONE', #11156, 1000.000000000000000 ) ;
#12272 = ORIENTED_EDGE ( 'NONE', *, *, #4676, .F. ) ;
#12273 = DIRECTION ( 'NONE',  ( 1.000000000000000000, 0.000000000000000000, 0.000000000000000000 ) ) ;
#12274 = SURFACE_STYLE_FILL_AREA ( #9895 ) ;
#12275 = ORIENTED_EDGE ( 'NONE', *, *, #13726, .T. ) ;
#12276 = CARTESIAN_POINT ( 'NONE',  ( 32.06294366074496338, -42.50536573064421475, -13.00000000000000178 ) ) ;
#12277 = DIRECTION ( 'NONE',  ( 0.5000000000000009992, -6.123233995736778362E-17, 0.8660254037844380415 ) ) ;
#12278 = DIRECTION ( 'NONE',  ( 1.000000000000000000, 0.000000000000000000, 0.000000000000000000 ) ) ;
#12279 = ORIENTED_EDGE ( 'NONE', *, *, #6824, .F. ) ;
#12280 = ORIENTED_EDGE ( 'NONE', *, *, #6005, .F. ) ;
#12281 = ORIENTED_EDGE ( 'NONE', *, *, #11221, .F. ) ;
#12282 = AXIS2_PLACEMENT_3D ( 'NONE', #4754, #3541, #7853 ) ;
#12283 = DIRECTION ( 'NONE',  ( 0.000000000000000000, 0.000000000000000000, 1.000000000000000000 ) ) ;
#12284 = CARTESIAN_POINT ( 'NONE',  ( 31.50188236243967665, 102.2577520262375828, 11.65984174646773930 ) ) ;
#12285 = DIRECTION ( 'NONE',  ( 0.000000000000000000, 0.000000000000000000, -1.000000000000000000 ) ) ;
#12286 = EDGE_LOOP ( 'NONE', ( #13824, #9871, #14949, #7252, #2037 ) ) ;
#12287 = ORIENTED_EDGE ( 'NONE', *, *, #8531, .T. ) ;
#12288 = ORIENTED_EDGE ( 'NONE', *, *, #3711, .F. ) ;
#12289 = AXIS2_PLACEMENT_3D ( 'NONE', #3444, #6985, #4656 ) ;
#12290 = CARTESIAN_POINT ( 'NONE',  ( -52.83493649053890806, 0.000000000000000000, -11.74999999999999822 ) ) ;
#12291 = EDGE_CURVE ( 'NONE', #5635, #11081, #4463, .T. ) ;
#12292 = DIRECTION ( 'NONE',  ( -0.000000000000000000, -0.000000000000000000, 1.000000000000000000 ) ) ;
#12293 = EDGE_CURVE ( 'NONE', #9491, #7296, #10057, .T. ) ;
#12294 = CARTESIAN_POINT ( 'NONE',  ( -12.39897948556635754, 100.2360479454198696, -16.00000000000000000 ) ) ;
#12295 = CARTESIAN_POINT ( 'NONE',  ( 12.50000000000000000, 40.62019202317980415, 16.00000000000000000 ) ) ;
#12296 = DIRECTION ( 'NONE',  ( 0.000000000000000000, 0.000000000000000000, 1.000000000000000000 ) ) ;
#12297 = ORIENTED_EDGE ( 'NONE', *, *, #8217, .T. ) ;
#12298 = DIRECTION ( 'NONE',  ( 1.000000000000000000, 0.000000000000000000, 0.000000000000000000 ) ) ;
#12299 = AXIS2_PLACEMENT_3D ( 'NONE', #9788, #14439, #1830 ) ;
#12300 = ORIENTED_EDGE ( 'NONE', *, *, #14805, .F. ) ;
#12301 = EDGE_CURVE ( 'NONE', #7513, #13798, #1549, .T. ) ;
#12302 = ORIENTED_EDGE ( 'NONE', *, *, #6328, .F. ) ;
#12303 = CARTESIAN_POINT ( 'NONE',  ( -29.70588235294120238, 96.53269163155678712, 11.33021639467930797 ) ) ;
#12304 = PRODUCT_RELATED_PRODUCT_CATEGORY ( 'part', '', ( #6312 ) ) ;
#12305 = CARTESIAN_POINT ( 'NONE',  ( 0.000000000000000000, 0.000000000000000000, 16.00000000000000000 ) ) ;
#12306 = UNCERTAINTY_MEASURE_WITH_UNIT (LENGTH_MEASURE( 1.000000000000000082E-05 ), #6967, 'distance_accuracy_value', 'NONE');
#12307 = DIRECTION ( 'NONE',  ( 0.000000000000000000, 0.000000000000000000, -1.000000000000000000 ) ) ;
#12308 = DIRECTION ( 'NONE',  ( 0.000000000000000000, 0.000000000000000000, 1.000000000000000000 ) ) ;
#12309 = EDGE_CURVE ( 'NONE', #5327, #4514, #8326, .T. ) ;
#12310 = DIRECTION ( 'NONE',  ( -1.000000000000000000, 0.000000000000000000, 0.000000000000000000 ) ) ;
#12311 = EDGE_LOOP ( 'NONE', ( #3828, #14813, #14876, #188, #4259, #6133 ) ) ;
#12312 = CARTESIAN_POINT ( 'NONE',  ( -71.53347797788819662, -69.16568774265570596, -8.000000000000000000 ) ) ;
#12313 = APPLICATION_CONTEXT ( 'automotive_design' ) ;
#12314 = DIRECTION ( 'NONE',  ( -1.000000000000000000, 0.000000000000000000, 0.000000000000000000 ) ) ;
#12315 = CARTESIAN_POINT ( 'NONE',  ( 0.3461262719736162841, -4.658553426539305597, -3.671615880910381158 ) ) ;
#12316 = VERTEX_POINT ( 'NONE', #726 ) ;
#12317 = DIRECTION ( 'NONE',  ( -1.000000000000000000, 0.000000000000000000, 0.000000000000000000 ) ) ;
#12318 = CIRCLE ( 'NONE', #3594, 50.00000000000000000 ) ;
#12319 = ORIENTED_EDGE ( 'NONE', *, *, #12870, .F. ) ;
#12320 = DIRECTION ( 'NONE',  ( 0.000000000000000000, 0.000000000000000000, -1.000000000000000000 ) ) ;
#12321 = ORIENTED_EDGE ( 'NONE', *, *, #9613, .F. ) ;
#12322 = ORIENTED_EDGE ( 'NONE', *, *, #12870, .T. ) ;
#12323 = CARTESIAN_POINT ( 'NONE',  ( 37.12029293941379393, 89.61631465359479876, -13.00000000000000178 ) ) ;
#12324 = CARTESIAN_POINT ( 'NONE',  ( 51.19406879332056093, 13.71740939043382745, -13.00000000000000178 ) ) ;
#12325 = CARTESIAN_POINT ( 'NONE',  ( -7.383907457637922889, -52.72775723226778410, -13.00000000000000178 ) ) ;
#12326 = CARTESIAN_POINT ( 'NONE',  ( -22.33583958711380646, -30.74264578624812927, -28.00000000000000000 ) ) ;
#12327 = DIRECTION ( 'NONE',  ( 1.000000000000000000, 0.000000000000000000, 0.000000000000000000 ) ) ;
#12328 = DIRECTION ( 'NONE',  ( 0.000000000000000000, 0.000000000000000000, 1.000000000000000000 ) ) ;
#12329 = ADVANCED_FACE ( 'NONE', ( #4076 ), #7546, .T. ) ;
#12330 = EDGE_LOOP ( 'NONE', ( #15023, #7298, #280, #13796, #14097, #3614, #5257, #6050, #5181, #5897 ) ) ;
#12331 = EDGE_CURVE ( 'NONE', #12974, #2645, #7353, .T. ) ;
#12332 = DIRECTION ( 'NONE',  ( -0.000000000000000000, -0.000000000000000000, -1.000000000000000000 ) ) ;
#12333 = DIRECTION ( 'NONE',  ( 1.000000000000000000, 0.000000000000000000, 0.000000000000000000 ) ) ;
#12334 = ADVANCED_FACE ( 'NONE', ( #7701 ), #570, .T. ) ;
#12335 = DIRECTION ( 'NONE',  ( 0.000000000000000000, 0.000000000000000000, -1.000000000000000000 ) ) ;
#12336 = VERTEX_POINT ( 'NONE', #6549 ) ;
#12337 = ORIENTED_EDGE ( 'NONE', *, *, #12830, .F. ) ;
#12338 = EDGE_CURVE ( 'NONE', #14269, #11532, #3240, .T. ) ;
#12339 = CYLINDRICAL_SURFACE ( 'NONE', #10221, 0.5000000000000043299 ) ;
#12340 = ORIENTED_EDGE ( 'NONE', *, *, #1398, .T. ) ;
#12341 = CARTESIAN_POINT ( 'NONE',  ( -25.00000000000000000, 81.24038404635962252, -23.50000000000000000 ) ) ;
#12342 = DIRECTION ( 'NONE',  ( 1.000000000000000000, 0.000000000000000000, 0.000000000000000000 ) ) ;
#12343 = DIRECTION ( 'NONE',  ( -0.000000000000000000, -0.000000000000000000, 1.000000000000000000 ) ) ;
#12344 = CARTESIAN_POINT ( 'NONE',  ( -9.706953719245875689, -57.06275842387046993, -13.00000000000000178 ) ) ;
#12345 = ORIENTED_EDGE ( 'NONE', *, *, #2481, .F. ) ;
#12346 = EDGE_LOOP ( 'NONE', ( #8275, #2004, #12923, #4223, #14098, #9907, #4926, #12233, #4024, #3730, #12925 ) ) ;
#12347 = EDGE_CURVE ( 'NONE', #10604, #10117, #3493, .T. ) ;
#12348 = CARTESIAN_POINT ( 'NONE',  ( 0.000000000000000000, 4.618802153517009401, -3.504269196027870237 ) ) ;
#12349 = DIRECTION ( 'NONE',  ( 0.000000000000000000, 0.000000000000000000, -1.000000000000000000 ) ) ;
#12350 = CARTESIAN_POINT ( 'NONE',  ( 25.00000000000000000, 81.24038404635960831, -23.50000000000000000 ) ) ;
#12351 = ORIENTED_EDGE ( 'NONE', *, *, #9204, .T. ) ;
#12352 = CIRCLE ( 'NONE', #15019, 59.50000000000000000 ) ;
#12353 = VERTEX_POINT ( 'NONE', #659 ) ;
#12354 = VERTEX_POINT ( 'NONE', #5281 ) ;
#12355 = DIRECTION ( 'NONE',  ( 1.000000000000000000, 0.000000000000000000, 0.000000000000000000 ) ) ;
#12356 = CARTESIAN_POINT ( 'NONE',  ( 49.57224306869053976, -6.526309611002402811, -8.000000000000000000 ) ) ;
#12357 = AXIS2_PLACEMENT_3D ( 'NONE', #9397, #9328, #4563 ) ;
#12358 = ORIENTED_EDGE ( 'NONE', *, *, #12594, .F. ) ;
#12359 = CARTESIAN_POINT ( 'NONE',  ( -32.26435573746199736, 42.04772703543562073, 8.000000000000000000 ) ) ;
#12360 = LINE ( 'NONE', #1958, #1968 ) ;
#12361 = ORIENTED_EDGE ( 'NONE', *, *, #3839, .F. ) ;
#12362 = CARTESIAN_POINT ( 'NONE',  ( 2.855764796983345288, -2.970025579236424296, -0.09382832055446289898 ) ) ;
#12363 = ORIENTED_EDGE ( 'NONE', *, *, #13081, .T. ) ;
#12364 = EDGE_CURVE ( 'NONE', #9738, #9553, #6046, .T. ) ;
#12365 = AXIS2_PLACEMENT_3D ( 'NONE', #2603, #7221, #3900 ) ;
#12366 = ORIENTED_EDGE ( 'NONE', *, *, #1250, .T. ) ;
#12367 = DIRECTION ( 'NONE',  ( 0.000000000000000000, -1.000000000000000000, 0.000000000000000000 ) ) ;
#12368 = CIRCLE ( 'NONE', #5806, 100.0000000000000000 ) ;
#12369 = EDGE_CURVE ( 'NONE', #1906, #3649, #8565, .T. ) ;
#12370 = AXIS2_PLACEMENT_3D ( 'NONE', #14925, #11730, #13782 ) ;
#12371 = EDGE_CURVE ( 'NONE', #4717, #14193, #14387, .T. ) ;
#12372 = AXIS2_PLACEMENT_3D ( 'NONE', #6586, #12375, #13363 ) ;
#12373 = CARTESIAN_POINT ( 'NONE',  ( 22.05882352941176094, 71.68269180561141241, -23.50000000000000000 ) ) ;
#12374 = DIRECTION ( 'NONE',  ( 1.000000000000000000, 0.000000000000000000, 0.000000000000000000 ) ) ;
#12375 = DIRECTION ( 'NONE',  ( -0.000000000000000000, -0.000000000000000000, -1.000000000000000000 ) ) ;
#12376 = AXIS2_PLACEMENT_3D ( 'NONE', #5625, #13599, #14824 ) ;
#12377 = LINE ( 'NONE', #2964, #9185 ) ;
#12378 = ORIENTED_EDGE ( 'NONE', *, *, #5636, .F. ) ;
#12379 = AXIS2_PLACEMENT_3D ( 'NONE', #3324, #6789, #10144 ) ;
#12380 = CARTESIAN_POINT ( 'NONE',  ( 5.000000000000004441, 0.000000000000000000, 2.775557561562891351E-14 ) ) ;
#12381 = AXIS2_PLACEMENT_3D ( 'NONE', #1368, #7189, #5979 ) ;
#12382 = CARTESIAN_POINT ( 'NONE',  ( -12.86891638962156215, 56.43380494353993271, -10.50000000000000000 ) ) ;
#12383 = DIRECTION ( 'NONE',  ( 0.000000000000000000, 0.000000000000000000, 1.000000000000000000 ) ) ;
#12384 = ORIENTED_EDGE ( 'NONE', *, *, #10885, .F. ) ;
#12385 = FACE_OUTER_BOUND ( 'NONE', #10898, .T. ) ;
#12386 = EDGE_CURVE ( 'NONE', #7029, #7912, #11989, .T. ) ;
#12387 = ADVANCED_FACE ( 'NONE', ( #11518 ), #9364, .F. ) ;
#12388 =( GEOMETRIC_REPRESENTATION_CONTEXT ( 3 ) GLOBAL_UNCERTAINTY_ASSIGNED_CONTEXT ( ( #12306 ) ) GLOBAL_UNIT_ASSIGNED_CONTEXT ( ( #6967, #11626, #9399 ) ) REPRESENTATION_CONTEXT ( 'NONE', 'WORKASPACE' ) );
#12389 = AXIS2_PLACEMENT_3D ( 'NONE', #5683, #2274, #13816 ) ;
#12390 = FACE_BOUND ( 'NONE', #1498, .T. ) ;
#12391 = ORIENTED_EDGE ( 'NONE', *, *, #6354, .F. ) ;
#12392 = DIRECTION ( 'NONE',  ( -0.000000000000000000, -0.000000000000000000, -1.000000000000000000 ) ) ;
#12393 = AXIS2_PLACEMENT_3D ( 'NONE', #10891, #9661, #1566 ) ;
#12394 = ORIENTED_EDGE ( 'NONE', *, *, #6983, .F. ) ;
#12395 = CARTESIAN_POINT ( 'NONE',  ( 0.000000000000000000, 0.000000000000000000, -10.50000000000000000 ) ) ;
#12396 = DIRECTION ( 'NONE',  ( 1.000000000000000000, -0.000000000000000000, -0.000000000000000000 ) ) ;
#12397 = CARTESIAN_POINT ( 'NONE',  ( 37.02125851216354846, -90.10640870805738700, -10.50000000000000000 ) ) ;
#12398 = LINE ( 'NONE', #11264, #710 ) ;
#12399 = DIRECTION ( 'NONE',  ( -0.000000000000000000, -0.000000000000000000, 1.000000000000000000 ) ) ;
#12400 = SURFACE_SIDE_STYLE ('',( #12482 ) ) ;
#12401 = AXIS2_PLACEMENT_3D ( 'NONE', #678, #600, #11148 ) ;
#12402 = ORIENTED_EDGE ( 'NONE', *, *, #11458, .F. ) ;
#12403 = FACE_OUTER_BOUND ( 'NONE', #9074, .T. ) ;
#12404 = CIRCLE ( 'NONE', #1217, 59.50000000000000000 ) ;
#12405 = DIRECTION ( 'NONE',  ( -1.000000000000000000, 0.000000000000000000, 0.000000000000000000 ) ) ;
#12406 = CIRCLE ( 'NONE', #11928, 3.000000000000002665 ) ;
#12407 = FACE_OUTER_BOUND ( 'NONE', #7963, .T. ) ;
#12408 = CARTESIAN_POINT ( 'NONE',  ( 35.00000000000000000, 81.24038404635960831, -23.50000000000000000 ) ) ;
#12409 = ORIENTED_EDGE ( 'NONE', *, *, #5416, .F. ) ;
#12410 = LINE ( 'NONE', #2005, #10947 ) ;
#12411 = ORIENTED_EDGE ( 'NONE', *, *, #6543, .F. ) ;
#12412 = EDGE_CURVE ( 'NONE', #9388, #13753, #4185, .T. ) ;
#12413 = DIRECTION ( 'NONE',  ( 0.000000000000000000, 0.000000000000000000, 1.000000000000000000 ) ) ;
#12414 = CYLINDRICAL_SURFACE ( 'NONE', #4426, 0.5000000000000004441 ) ;
#12415 = B_SPLINE_CURVE_WITH_KNOTS ( 'NONE', 3,
 ( #4727, #5705, #11712, #4572, #13990, #13920 ),
 .UNSPECIFIED., .F., .F.,
 ( 4, 2, 4 ),
 ( 0.002365888236227995083, 0.003551327329835084548, 0.004736766423442173579 ),
 .UNSPECIFIED. ) ;
#12416 = EDGE_CURVE ( 'NONE', #13772, #3549, #2022, .T. ) ;
#12417 = CYLINDRICAL_SURFACE ( 'NONE', #7748, 3.000000000000002665 ) ;
#12418 = CIRCLE ( 'NONE', #5858, 63.00000000000000000 ) ;
#12419 = CARTESIAN_POINT ( 'NONE',  ( 3.999999999999996447, -2.309401076758518911, -5.000000000000000888 ) ) ;
#12420 = CONTEXT_DEPENDENT_SHAPE_REPRESENTATION ( #3393, #9133 ) ;
#12421 = VERTEX_POINT ( 'NONE', #1037 ) ;
#12422 = VERTEX_POINT ( 'NONE', #15001 ) ;
#12423 = ORIENTED_EDGE ( 'NONE', *, *, #5612, .T. ) ;
#12424 =( REPRESENTATION_RELATIONSHIP ('NONE','NONE', #12187, #1232 ) REPRESENTATION_RELATIONSHIP_WITH_TRANSFORMATION ( #7135 )SHAPE_REPRESENTATION_RELATIONSHIP( ) );
#12425 = ADVANCED_FACE ( 'NONE', ( #4453 ), #10270, .T. ) ;
#12426 = DIRECTION ( 'NONE',  ( -0.000000000000000000, 1.000000000000000000, 0.000000000000000000 ) ) ;
#12427 = CARTESIAN_POINT ( 'NONE',  ( 37.21932736666271779, -89.12622059913267947, -10.50000000000000000 ) ) ;
#12428 = CARTESIAN_POINT ( 'NONE',  ( 33.48561063518626923, -47.21331623427104063, -10.50000000000000000 ) ) ;
#12429 = VERTEX_POINT ( 'NONE', #10286 ) ;
#12430 = AXIS2_PLACEMENT_3D ( 'NONE', #14609, #14523, #10034 ) ;
#12431 = VERTEX_POINT ( 'NONE', #14930 ) ;
#12432 = EDGE_CURVE ( 'NONE', #7912, #6631, #13927, .T. ) ;
#12433 = ORIENTED_EDGE ( 'NONE', *, *, #7488, .F. ) ;
#12434 = EDGE_CURVE ( 'NONE', #11559, #12743, #11250, .T. ) ;
#12435 = CARTESIAN_POINT ( 'NONE',  ( 0.000000000000000000, 0.000000000000000000, 0.000000000000000000 ) ) ;
#12436 = AXIS2_PLACEMENT_3D ( 'NONE', #3317, #8228, #5734 ) ;
#12437 = CARTESIAN_POINT ( 'NONE',  ( -3.492805317593278058, 46.55633131742322917, -10.50000000000000000 ) ) ;
#12438 = FILL_AREA_STYLE_COLOUR ( '', #988 ) ;
#12439 = CARTESIAN_POINT ( 'NONE',  ( -31.47058823529412663, 102.2673069760056421, -26.00000000000000000 ) ) ;
#12440 = ORIENTED_EDGE ( 'NONE', *, *, #6099, .T. ) ;
#12441 = CARTESIAN_POINT ( 'NONE',  ( 23.51438936481372366, 47.21331623427104063, 8.000000000000000000 ) ) ;
#12442 = PLANE ( 'NONE',  #4895 ) ;
#12443 = ORIENTED_EDGE ( 'NONE', *, *, #6274, .F. ) ;
#12444 = EDGE_CURVE ( 'NONE', #2878, #11690, #957, .T. ) ;
#12445 = CARTESIAN_POINT ( 'NONE',  ( 1.674280531759317014, -94.51066581171355097, -13.00000000000000178 ) ) ;
#12446 = AXIS2_PLACEMENT_3D ( 'NONE', #8317, #5132, #351 ) ;
#12447 = ORIENTED_EDGE ( 'NONE', *, *, #441, .T. ) ;
#12448 = CIRCLE ( 'NONE', #10498, 0.5000000000000004441 ) ;
#12449 = ORIENTED_EDGE ( 'NONE', *, *, #10073, .T. ) ;
#12450 = CARTESIAN_POINT ( 'NONE',  ( 25.00000000000000000, 81.24038404635960831, 26.00000000000000000 ) ) ;
#12451 = AXIS2_PLACEMENT_3D ( 'NONE', #7367, #6221, #14357 ) ;
#12452 = DIRECTION ( 'NONE',  ( -0.000000000000000000, -0.000000000000000000, -1.000000000000000000 ) ) ;
#12453 = CARTESIAN_POINT ( 'NONE',  ( 6.917888187663118416, 52.54657765281190507, -10.50000000000000000 ) ) ;
#12454 = AXIS2_PLACEMENT_3D ( 'NONE', #10732, #255, #3907 ) ;
#12455 = CARTESIAN_POINT ( 'NONE',  ( 0.000000000000000000, 0.000000000000000000, 10.50000000000000000 ) ) ;
#12456 = CARTESIAN_POINT ( 'NONE',  ( -27.94117647058823550, 90.79807628710781842, -23.50000000000000000 ) ) ;
#12457 = DIRECTION ( 'NONE',  ( 0.000000000000000000, 0.000000000000000000, 1.000000000000000000 ) ) ;
#12458 = VECTOR ( 'NONE', #10902, 1000.000000000000000 ) ;
#12459 = ORIENTED_EDGE ( 'NONE', *, *, #10787, .T. ) ;
#12460 = CYLINDRICAL_SURFACE ( 'NONE', #509, 57.00000000000000000 ) ;
#12461 = AXIS2_PLACEMENT_3D ( 'NONE', #14445, #859, #13298 ) ;
#12462 = DIRECTION ( 'NONE',  ( 1.000000000000000000, -1.749300984178292964E-15, 0.000000000000000000 ) ) ;
#12463 = CYLINDRICAL_SURFACE ( 'NONE', #10684, 3.000000000000002665 ) ;
#12464 = CIRCLE ( 'NONE', #10516, 3.000000000000002665 ) ;
#12465 = ORIENTED_EDGE ( 'NONE', *, *, #10283, .F. ) ;
#12466 = DIRECTION ( 'NONE',  ( 0.000000000000000000, 0.000000000000000000, -1.000000000000000000 ) ) ;
#12467 = ORIENTED_EDGE ( 'NONE', *, *, #11019, .F. ) ;
#12468 = CARTESIAN_POINT ( 'NONE',  ( 26.49999999999971578, 45.89934640057541060, 10.49999999999999822 ) ) ;
#12469 = ORIENTED_EDGE ( 'NONE', *, *, #6501, .F. ) ;
#12470 = CARTESIAN_POINT ( 'NONE',  ( 0.000000000000000000, 0.000000000000000000, 8.000000000000000000 ) ) ;
#12471 = CARTESIAN_POINT ( 'NONE',  ( -12.39897948556635754, 94.18739463280904545, -16.00000000000000000 ) ) ;
#12472 = DIRECTION ( 'NONE',  ( 1.000000000000000000, 0.000000000000000000, 0.000000000000000000 ) ) ;
#12473 = CARTESIAN_POINT ( 'NONE',  ( 0.000000000000000000, 0.000000000000000000, 8.000000000000000000 ) ) ;
#12474 = VECTOR ( 'NONE', #439, 1000.000000000000000 ) ;
#12475 = EDGE_CURVE ( 'NONE', #8389, #9955, #5574, .T. ) ;
#12476 = AXIS2_PLACEMENT_3D ( 'NONE', #7009, #5741, #14944 ) ;
#12477 = CARTESIAN_POINT ( 'NONE',  ( 22.33583958711425055, -30.74264578624780597, -28.00000000000000000 ) ) ;
#12478 = EDGE_CURVE ( 'NONE', #11670, #14615, #5664, .T. ) ;
#12479 = CARTESIAN_POINT ( 'NONE',  ( -7.500000000000000000, 74.62405778299650194, -20.00000000000000000 ) ) ;
#12480 = EDGE_CURVE ( 'NONE', #9297, #669, #7593, .T. ) ;
#12481 = EDGE_CURVE ( 'NONE', #12042, #12813, #1071, .T. ) ;
#12482 = SURFACE_STYLE_FILL_AREA ( #7832 ) ;
#12483 = ORIENTED_EDGE ( 'NONE', *, *, #3109, .F. ) ;
#12484 = CARTESIAN_POINT ( 'NONE',  ( 7.500000000000000888, 94.70348462437907244, -20.00000000000000000 ) ) ;
#12485 = CARTESIAN_POINT ( 'NONE',  ( 42.04772703543530099, 32.26435573746242369, 8.000000000000000000 ) ) ;
#12486 = AXIS2_PLACEMENT_3D ( 'NONE', #13932, #12708, #1104 ) ;
#12487 = AXIS2_PLACEMENT_3D ( 'NONE', #14552, #2711, #2858 ) ;
#12488 = FACE_OUTER_BOUND ( 'NONE', #9088, .T. ) ;
#12489 = AXIS2_PLACEMENT_3D ( 'NONE', #10260, #10404, #4646 ) ;
#12490 = CIRCLE ( 'NONE', #14670, 63.00000000000000000 ) ;
#12491 = CARTESIAN_POINT ( 'NONE',  ( -31.05588327715806329, 44.79355920668842828, -8.000000000000000000 ) ) ;
#12492 = VERTEX_POINT ( 'NONE', #2316 ) ;
#12493 = DIRECTION ( 'NONE',  ( 0.000000000000000000, 0.000000000000000000, 1.000000000000000000 ) ) ;
#12494 = ORIENTED_EDGE ( 'NONE', *, *, #4809, .F. ) ;
#12495 = DIRECTION ( 'NONE',  ( 0.000000000000000000, 0.000000000000000000, 1.000000000000000000 ) ) ;
#12496 = LINE ( 'NONE', #4225, #8043 ) ;
#12497 = ORIENTED_EDGE ( 'NONE', *, *, #9520, .F. ) ;
#12498 = CARTESIAN_POINT ( 'NONE',  ( 12.33783400350010950, 106.2863213744706172, -16.30550365830425719 ) ) ;
#12499 = DIRECTION ( 'NONE',  ( 1.000000000000000000, 1.765157221169382931E-15, 0.000000000000000000 ) ) ;
#12500 = ORIENTED_EDGE ( 'NONE', *, *, #12526, .F. ) ;
#12501 = AXIS2_PLACEMENT_3D ( 'NONE', #1499, #8466, #11757 ) ;
#12502 = EDGE_CURVE ( 'NONE', #14249, #5898, #5892, .T. ) ;
#12503 = ORIENTED_EDGE ( 'NONE', *, *, #11021, .T. ) ;
#12504 = FACE_OUTER_BOUND ( 'NONE', #7059, .T. ) ;
#12505 = CARTESIAN_POINT ( 'NONE',  ( 31.62605012285506945, 102.2189371620064833, 12.30800327571618880 ) ) ;
#12506 = EDGE_CURVE ( 'NONE', #2474, #7240, #3309, .T. ) ;
#12507 = CARTESIAN_POINT ( 'NONE',  ( 0.000000000000000000, 0.000000000000000000, -11.74999999999999822 ) ) ;
#12508 = ORIENTED_EDGE ( 'NONE', *, *, #14880, .F. ) ;
#12509 = AXIS2_PLACEMENT_3D ( 'NONE', #916, #4481, #2187 ) ;
#12510 = EDGE_LOOP ( 'NONE', ( #3598, #8730, #10599, #11369, #7222, #6211 ) ) ;
#12511 = ORIENTED_EDGE ( 'NONE', *, *, #11867, .F. ) ;
#12512 = DIRECTION ( 'NONE',  ( 0.000000000000000000, 0.000000000000000000, -1.000000000000000000 ) ) ;
#12513 = DIRECTION ( 'NONE',  ( -0.000000000000000000, -0.000000000000000000, 1.000000000000000000 ) ) ;
#12514 = CARTESIAN_POINT ( 'NONE',  ( 4.211140560182194292, -2.431303136016555122, -3.745885042887437510 ) ) ;
#12515 = DIRECTION ( 'NONE',  ( -0.000000000000000000, -0.000000000000000000, 1.000000000000000000 ) ) ;
#12516 = AXIS2_PLACEMENT_3D ( 'NONE', #2174, #13961, #3473 ) ;
#12517 = CIRCLE ( 'NONE', #7898, 63.00000000000000000 ) ;
#12518 = ORIENTED_EDGE ( 'NONE', *, *, #4427, .T. ) ;
#12519 = CARTESIAN_POINT ( 'NONE',  ( 12.94095225512608494, -48.29629131445340562, -8.000000000000000000 ) ) ;
#12520 = CARTESIAN_POINT ( 'NONE',  ( -9.706953719245875689, -57.06275842387046993, 8.000000000000000000 ) ) ;
#12521 = EDGE_LOOP ( 'NONE', ( #3561, #12820, #10388, #8041 ) ) ;
#12523 = EDGE_CURVE ( 'NONE', #13856, #2085, #13663, .T. ) ;
#12522 = CARTESIAN_POINT ( 'NONE',  ( 0.000000000000000000, 0.000000000000000000, -4.000000000000000000 ) ) ;
#12524 = EDGE_CURVE ( 'NONE', #13552, #11211, #334, .T. ) ;
#12525 = ORIENTED_EDGE ( 'NONE', *, *, #12047, .F. ) ;
#12526 = EDGE_CURVE ( 'NONE', #1196, #1622, #6623, .T. ) ;
#12527 = ORIENTED_EDGE ( 'NONE', *, *, #7924, .T. ) ;
#12528 = DIRECTION ( 'NONE',  ( -1.000000000000000000, 0.000000000000000000, 0.000000000000000000 ) ) ;
#12529 = CIRCLE ( 'NONE', #3314, 50.00000000000000000 ) ;
#12530 = ORIENTED_EDGE ( 'NONE', *, *, #1022, .F. ) ;
#12531 = DIRECTION ( 'NONE',  ( 0.000000000000000000, 0.000000000000000000, 1.000000000000000000 ) ) ;
#12532 = ADVANCED_FACE ( 'NONE', ( #10647 ), #9647, .F. ) ;
#12533 = DIRECTION ( 'NONE',  ( 0.000000000000000000, 0.000000000000000000, -1.000000000000000000 ) ) ;
#12534 = DIRECTION ( 'NONE',  ( -0.000000000000000000, -0.000000000000000000, 1.000000000000000000 ) ) ;
#12535 = CARTESIAN_POINT ( 'NONE',  ( 22.05882352941176094, 71.68269180561141241, -23.50000000000000000 ) ) ;
#12536 = VERTEX_POINT ( 'NONE', #14297 ) ;
#12537 = AXIS2_PLACEMENT_3D ( 'NONE', #9812, #2989, #713 ) ;
#12538 = FACE_BOUND ( 'NONE', #9688, .T. ) ;
#12539 = PRODUCT_DEFINITION_SHAPE ( 'NONE', 'NONE',  #15034 ) ;
#12540 = EDGE_CURVE ( 'NONE', #13630, #5022, #89, .T. ) ;
#12541 = DIRECTION ( 'NONE',  ( -0.000000000000000000, -0.000000000000000000, -1.000000000000000000 ) ) ;
#12542 = CARTESIAN_POINT ( 'NONE',  ( 36.70371619500516402, 89.33979373934434420, -13.00000000000000178 ) ) ;
#12543 = ORIENTED_EDGE ( 'NONE', *, *, #9624, .T. ) ;
#12544 = CARTESIAN_POINT ( 'NONE',  ( -4.211140560182194292, -2.431303136016555122, -3.745885042887437510 ) ) ;
#12545 = VERTEX_POINT ( 'NONE', #14076 ) ;
#12546 = DIRECTION ( 'NONE',  ( -1.000000000000000000, 9.329605248950895679E-16, 0.000000000000000000 ) ) ;
#12547 = FACE_OUTER_BOUND ( 'NONE', #13874, .T. ) ;
#12548 = CARTESIAN_POINT ( 'NONE',  ( 49.00442420935993226, -30.80502811811213704, -8.000000000000000000 ) ) ;
#12549 = DIRECTION ( 'NONE',  ( 1.000000000000000000, 0.000000000000000000, 0.000000000000000000 ) ) ;
#12550 = DIRECTION ( 'NONE',  ( -0.000000000000000000, -0.000000000000000000, 1.000000000000000000 ) ) ;
#12551 = CYLINDRICAL_SURFACE ( 'NONE', #3407, 63.00000000000000000 ) ;
#12552 = CARTESIAN_POINT ( 'NONE',  ( -8.635752201752492141, 74.50170565226535757, -19.87768552833457392 ) ) ;
#12553 = DIRECTION ( 'NONE',  ( 0.000000000000000000, 0.000000000000000000, -1.000000000000000000 ) ) ;
#12554 = EDGE_LOOP ( 'NONE', ( #10296, #795, #6448, #4616 ) ) ;
#12555 = DIRECTION ( 'NONE',  ( 1.000000000000000000, 0.000000000000000000, 0.000000000000000000 ) ) ;
#12556 = DIRECTION ( 'NONE',  ( -1.000000000000000000, 0.000000000000000000, 0.000000000000000000 ) ) ;
#12557 = AXIS2_PLACEMENT_3D ( 'NONE', #2113, #5530, #6654 ) ;
#12558 = PLANE ( 'NONE',  #8309 ) ;
#12559 = CARTESIAN_POINT ( 'NONE',  ( -4.121772567811602173, -51.45950017607692217, -13.00000000000000178 ) ) ;
#12560 = ORIENTED_EDGE ( 'NONE', *, *, #7585, .T. ) ;
#12561 = EDGE_CURVE ( 'NONE', #297, #8589, #11500, .T. ) ;
#12562 = DIRECTION ( 'NONE',  ( 1.000000000000000000, 0.000000000000000000, 0.000000000000000000 ) ) ;
#12563 = EDGE_CURVE ( 'NONE', #1453, #11466, #2276, .T. ) ;
#12564 = ORIENTED_EDGE ( 'NONE', *, *, #9787, .T. ) ;
#12565 = DIRECTION ( 'NONE',  ( 1.000000000000000000, 0.000000000000000000, 0.000000000000000000 ) ) ;
#12566 = PLANE ( 'NONE',  #779 ) ;
#12567 = CIRCLE ( 'NONE', #11029, 100.0000000000000000 ) ;
#12568 = DIRECTION ( 'NONE',  ( 1.000000000000000000, 0.000000000000000000, 0.000000000000000000 ) ) ;
#12569 = DIRECTION ( 'NONE',  ( -0.000000000000000000, -0.000000000000000000, -1.000000000000000000 ) ) ;
#12570 = ORIENTED_EDGE ( 'NONE', *, *, #13823, .F. ) ;
#12571 = ORIENTED_EDGE ( 'NONE', *, *, #2124, .T. ) ;
#12572 = DIRECTION ( 'NONE',  ( 1.000000000000000000, 0.000000000000000000, 0.000000000000000000 ) ) ;
#12573 = CARTESIAN_POINT ( 'NONE',  ( 2.500000000000002220, -1.178949249685208533, 2.042000000000002036 ) ) ;
#12574 = EDGE_CURVE ( 'NONE', #8815, #11525, #6014, .T. ) ;
#12575 = DIRECTION ( 'NONE',  ( 0.000000000000000000, 0.000000000000000000, -1.000000000000000000 ) ) ;
#12576 = VERTEX_POINT ( 'NONE', #5112 ) ;
#12577 = ORIENTED_EDGE ( 'NONE', *, *, #2480, .T. ) ;
#12578 = ADVANCED_FACE ( 'NONE', ( #14154 ), #12040, .T. ) ;
#12579 = ORIENTED_EDGE ( 'NONE', *, *, #3943, .F. ) ;
#12580 = CARTESIAN_POINT ( 'NONE',  ( 11.08463629228402603, 74.17659209477393745, 18.49742775384897087 ) ) ;
#12581 = LINE ( 'NONE', #2961, #1950 ) ;
#12582 = DIRECTION ( 'NONE',  ( -1.000000000000000000, 0.000000000000000000, 0.000000000000000000 ) ) ;
#12583 =( LENGTH_UNIT ( ) NAMED_UNIT ( * ) SI_UNIT ( .MILLI., .METRE. ) );
#12584 = DIRECTION ( 'NONE',  ( 0.000000000000000000, 0.000000000000000000, 1.000000000000000000 ) ) ;
#12585 = CARTESIAN_POINT ( 'NONE',  ( -49.54657765281192638, 6.917888187662934563, 8.000000000000000000 ) ) ;
#12586 = ORIENTED_EDGE ( 'NONE', *, *, #3575, .F. ) ;
#12587 = DIRECTION ( 'NONE',  ( 0.000000000000000000, 0.000000000000000000, -1.000000000000000000 ) ) ;
#12588 = DIRECTION ( 'NONE',  ( -0.000000000000000000, -0.000000000000000000, 1.000000000000000000 ) ) ;
#12589 = VERTEX_POINT ( 'NONE', #3608 ) ;
#12590 = ORIENTED_EDGE ( 'NONE', *, *, #2605, .F. ) ;
#12591 = PLANE ( 'NONE',  #8140 ) ;
#12592 = ORIENTED_EDGE ( 'NONE', *, *, #11259, .F. ) ;
#12593 = CARTESIAN_POINT ( 'NONE',  ( -7.500000000000000888, 61.74746958378133144, -20.00000000000000000 ) ) ;
#12594 = EDGE_CURVE ( 'NONE', #6415, #212, #1627, .T. ) ;
#12595 = VECTOR ( 'NONE', #7501, 1000.000000000000000 ) ;
#12596 = CARTESIAN_POINT ( 'NONE',  ( 0.000000000000000000, 0.000000000000000000, 0.000000000000000000 ) ) ;
#12597 = EDGE_CURVE ( 'NONE', #14933, #13551, #8097, .T. ) ;
#12598 = ADVANCED_FACE ( 'NONE', ( #8222 ), #9585, .F. ) ;
#12599 = CARTESIAN_POINT ( 'NONE',  ( -3.492805317593278058, 46.55633131742322917, -10.50000000000000000 ) ) ;
#12600 = CARTESIAN_POINT ( 'NONE',  ( -3.455068668934470733, 2.624017327439040592, -3.316620875263627699 ) ) ;
#12601 = DIRECTION ( 'NONE',  ( -0.000000000000000000, -0.000000000000000000, -1.000000000000000000 ) ) ;
#12602 = VERTEX_POINT ( 'NONE', #1551 ) ;
#12603 = PRESENTATION_LAYER_ASSIGNMENT (  '', '', ( #5077 ) ) ;
#12604 = CARTESIAN_POINT ( 'NONE',  ( -24.98583958711379793, -30.74264578624812927, -28.00000000000000000 ) ) ;
#12605 = AXIS2_PLACEMENT_3D ( 'NONE', #3106, #13504, #603 ) ;
#12606 = EDGE_CURVE ( 'NONE', #2333, #14343, #4237, .T. ) ;
#12607 = CARTESIAN_POINT ( 'NONE',  ( -13.35619814848797837, 51.53979475227131246, -10.50000000000000000 ) ) ;
#12608 = AXIS2_PLACEMENT_3D ( 'NONE', #11560, #6965, #2348 ) ;
#12609 = CARTESIAN_POINT ( 'NONE',  ( 7.500000000000007105, 85.00000000000000000, 46.00000000000000000 ) ) ;
#12610 = AXIS2_PLACEMENT_3D ( 'NONE', #10785, #13069, #4873 ) ;
#12611 = ORIENTED_EDGE ( 'NONE', *, *, #5967, .T. ) ;
#12612 = FACE_OUTER_BOUND ( 'NONE', #10309, .T. ) ;
#12613 = ORIENTED_EDGE ( 'NONE', *, *, #3984, .F. ) ;
#12614 = FACE_OUTER_BOUND ( 'NONE', #7862, .T. ) ;
#12615 = LINE ( 'NONE', #1089, #14077 ) ;
#12616 = EDGE_CURVE ( 'NONE', #4787, #11326, #11998, .T. ) ;
#12617 = AXIS2_PLACEMENT_3D ( 'NONE', #12836, #1302, #5 ) ;
#12618 = EDGE_CURVE ( 'NONE', #9852, #4454, #5189, .T. ) ;
#12619 = CARTESIAN_POINT ( 'NONE',  ( -7.383907457637922889, -52.72775723226778410, 10.49999999999999822 ) ) ;
#12620 = CARTESIAN_POINT ( 'NONE',  ( -50.84834283437000835, -14.07862063237876704, -13.00000000000000178 ) ) ;
#12621 = CARTESIAN_POINT ( 'NONE',  ( -37.12029293941441210, -89.61631465359452875, -13.00000000000000178 ) ) ;
#12622 = CIRCLE ( 'NONE', #10910, 0.5000000000000004441 ) ;
#12623 = FACE_OUTER_BOUND ( 'NONE', #13567, .T. ) ;
#12624 = CIRCLE ( 'NONE', #12867, 60.49999999999999289 ) ;
#12625 = ORIENTED_EDGE ( 'NONE', *, *, #7259, .T. ) ;
#12626 = CARTESIAN_POINT ( 'NONE',  ( -13.71740939043329277, 51.19406879332069593, -13.00000000000000178 ) ) ;
#12627 = CARTESIAN_POINT ( 'NONE',  ( 34.62083247296202160, 87.95718916809205723, -8.000000000000000000 ) ) ;
#12628 = AXIS2_PLACEMENT_3D ( 'NONE', #1069, #9248, #11694 ) ;
#12629 = DIRECTION ( 'NONE',  ( -1.000000000000000000, 0.000000000000000000, 0.000000000000000000 ) ) ;
#12630 = CIRCLE ( 'NONE', #5589, 0.5000000000000004441 ) ;
#12631 = DIRECTION ( 'NONE',  ( 0.000000000000000000, 0.000000000000000000, -1.000000000000000000 ) ) ;
#12632 = AXIS2_PLACEMENT_3D ( 'NONE', #9889, #489, #12188 ) ;
#12633 = VERTEX_POINT ( 'NONE', #8450 ) ;
#12634 = CARTESIAN_POINT ( 'NONE',  ( 68.58935777509475429, -68.58935777509547904, -13.00000000000000178 ) ) ;
#12635 = ORIENTED_EDGE ( 'NONE', *, *, #902, .F. ) ;
#12636 = CARTESIAN_POINT ( 'NONE',  ( -2.171643655288372887, 3.365003104552320323, 1.141800412898796857E-15 ) ) ;
#12637 = PLANE ( 'NONE',  #5393 ) ;
#12638 = AXIS2_PLACEMENT_3D ( 'NONE', #12908, #10549, #153 ) ;
#12639 = CIRCLE ( 'NONE', #8273, 59.50000000000000000 ) ;
#12640 = CARTESIAN_POINT ( 'NONE',  ( 29.51438936481373077, 47.21331623427104063, -8.000000000000000000 ) ) ;
#12641 = DIRECTION ( 'NONE',  ( 0.000000000000000000, -0.5000000000000012212, -0.8660254037844380415 ) ) ;
#12642 = ORIENTED_EDGE ( 'NONE', *, *, #8604, .T. ) ;
#12643 = CIRCLE ( 'NONE', #9231, 3.000000000000002665 ) ;
#12644 = ORIENTED_EDGE ( 'NONE', *, *, #8463, .F. ) ;
#12645 = VERTEX_POINT ( 'NONE', #7156 ) ;
#12646 = CIRCLE ( 'NONE', #6081, 60.50000000000000000 ) ;
#12647 = ORIENTED_EDGE ( 'NONE', *, *, #10561, .T. ) ;
#12648 = ORIENTED_EDGE ( 'NONE', *, *, #12412, .T. ) ;
#12649 = EDGE_CURVE ( 'NONE', #10590, #3770, #343, .T. ) ;
#12650 = DIRECTION ( 'NONE',  ( 0.000000000000000000, 0.000000000000000000, 1.000000000000000000 ) ) ;
#12651 = CARTESIAN_POINT ( 'NONE',  ( 0.000000000000000000, 0.000000000000000000, 0.000000000000000000 ) ) ;
#12652 = DIRECTION ( 'NONE',  ( 0.000000000000000000, 0.000000000000000000, 1.000000000000000000 ) ) ;
#12653 = ORIENTED_EDGE ( 'NONE', *, *, #2210, .T. ) ;
#12654 = AXIS2_PLACEMENT_3D ( 'NONE', #14614, #12553, #6756 ) ;
#12655 = ORIENTED_EDGE ( 'NONE', *, *, #11662, .T. ) ;
#12656 = EDGE_LOOP ( 'NONE', ( #7718, #10758, #5702, #4166 ) ) ;
#12657 = VECTOR ( 'NONE', #8910, 1000.000000000000000 ) ;
#12658 = CARTESIAN_POINT ( 'NONE',  ( 8.072319373765147077, 74.56485781596312279, 19.97535925451852989 ) ) ;
#12659 = CYLINDRICAL_SURFACE ( 'NONE', #3901, 95.00000000000001421 ) ;
#12660 = LINE ( 'NONE', #13731, #8313 ) ;
#12661 = DIRECTION ( 'NONE',  ( 0.000000000000000000, 0.000000000000000000, -1.000000000000000000 ) ) ;
#12662 = ORIENTED_EDGE ( 'NONE', *, *, #10242, .T. ) ;
#12663 = DIRECTION ( 'NONE',  ( -1.000000000000000000, 0.000000000000000000, 0.000000000000000000 ) ) ;
#12664 = ORIENTED_EDGE ( 'NONE', *, *, #1565, .T. ) ;
#12665 = EDGE_CURVE ( 'NONE', #1453, #5585, #11962, .T. ) ;
#12666 = ORIENTED_EDGE ( 'NONE', *, *, #11216, .F. ) ;
#12667 = EDGE_CURVE ( 'NONE', #11211, #5988, #12464, .T. ) ;
#12668 = EDGE_CURVE ( 'NONE', #2406, #1338, #8338, .T. ) ;
#12669 = CARTESIAN_POINT ( 'NONE',  ( -68.58935777509570642, -68.58935777509452691, -8.000000000000000000 ) ) ;
#12670 = CYLINDRICAL_SURFACE ( 'NONE', #681, 101.0000000000000284 ) ;
#12671 = AXIS2_PLACEMENT_3D ( 'NONE', #13242, #7224, #1548 ) ;
#12672 = EDGE_LOOP ( 'NONE', ( #3295, #755, #8491, #12127, #9208, #9978 ) ) ;
#12673 = ORIENTED_EDGE ( 'NONE', *, *, #12434, .T. ) ;
#12674 = DIRECTION ( 'NONE',  ( 1.000000000000000000, 0.000000000000000000, 0.000000000000000000 ) ) ;
#12675 = ORIENTED_EDGE ( 'NONE', *, *, #3818, .F. ) ;
#12676 = CIRCLE ( 'NONE', #6114, 59.50000000000000000 ) ;
#12677 = ORIENTED_EDGE ( 'NONE', *, *, #5409, .T. ) ;
#12678 = DIRECTION ( 'NONE',  ( 0.000000000000000000, 0.000000000000000000, 1.000000000000000000 ) ) ;
#12679 = DIRECTION ( 'NONE',  ( 0.000000000000000000, 0.000000000000000000, 1.000000000000000000 ) ) ;
#12680 = AXIS2_PLACEMENT_3D ( 'NONE', #12473, #8963, #707 ) ;
#12681 = DIRECTION ( 'NONE',  ( -0.000000000000000000, -0.000000000000000000, -1.000000000000000000 ) ) ;
#12682 = CARTESIAN_POINT ( 'NONE',  ( -49.00442420935969778, 30.80502811811250297, -13.00000000000000178 ) ) ;
#12683 = PLANE ( 'NONE',  #7245 ) ;
#12684 = ORIENTED_EDGE ( 'NONE', *, *, #4678, .F. ) ;
#12685 = CARTESIAN_POINT ( 'NONE',  ( 32.26435573746228158, -42.04772703543541468, 8.000000000000000000 ) ) ;
#12686 = CIRCLE ( 'NONE', #5411, 63.00000000000000000 ) ;
#12687 = CARTESIAN_POINT ( 'NONE',  ( -4.211140560182194292, 2.431303136016534250, -3.745885042887433958 ) ) ;
#12688 = ADVANCED_FACE ( 'NONE', ( #10957 ), #3071, .T. ) ;
#12689 = ORIENTED_EDGE ( 'NONE', *, *, #1034, .T. ) ;
#12690 = FACE_OUTER_BOUND ( 'NONE', #2972, .T. ) ;
#12691 = AXIS2_PLACEMENT_3D ( 'NONE', #4470, #2470, #5743 ) ;
#12692 = CARTESIAN_POINT ( 'NONE',  ( 33.83031011230895047, 95.16624652083665126, 15.96768307234234108 ) ) ;
#12693 = DIRECTION ( 'NONE',  ( 1.000000000000000000, 0.000000000000000000, 0.000000000000000000 ) ) ;
#12694 = CIRCLE ( 'NONE', #2751, 10.00000000000000355 ) ;
#12695 = DIRECTION ( 'NONE',  ( 0.000000000000000000, 0.000000000000000000, 1.000000000000000000 ) ) ;
#12696 = CARTESIAN_POINT ( 'NONE',  ( -8.154413083459852274, 106.6893057894985617, 19.96764870088428623 ) ) ;
#12697 = DIRECTION ( 'NONE',  ( -0.000000000000000000, -0.000000000000000000, 1.000000000000000000 ) ) ;
#12698 = LINE ( 'NONE', #10934, #12595 ) ;
#12699 = DIRECTION ( 'NONE',  ( -0.000000000000000000, -0.000000000000000000, 1.000000000000000000 ) ) ;
#12700 = AXIS2_PLACEMENT_3D ( 'NONE', #6234, #4897, #8382 ) ;
#12701 = ORIENTED_EDGE ( 'NONE', *, *, #14201, .T. ) ;
#12702 = FACE_OUTER_BOUND ( 'NONE', #3506, .T. ) ;
#12703 = DIRECTION ( 'NONE',  ( 1.000000000000000000, 0.000000000000000000, 0.000000000000000000 ) ) ;
#12704 = EDGE_CURVE ( 'NONE', #628, #11806, #13531, .T. ) ;
#12705 = EDGE_CURVE ( 'NONE', #4759, #8664, #8669, .T. ) ;
#12706 = FACE_OUTER_BOUND ( 'NONE', #6150, .T. ) ;
#12707 = ORIENTED_EDGE ( 'NONE', *, *, #7358, .T. ) ;
#12708 = DIRECTION ( 'NONE',  ( -0.000000000000000000, -0.000000000000000000, 1.000000000000000000 ) ) ;
#12709 = EDGE_LOOP ( 'NONE', ( #13609, #8878, #2389, #3222 ) ) ;
#12710 =( REPRESENTATION_RELATIONSHIP ('NONE','NONE', #12187, #8006 ) REPRESENTATION_RELATIONSHIP_WITH_TRANSFORMATION ( #13629 )SHAPE_REPRESENTATION_RELATIONSHIP( ) );
#12711 = CIRCLE ( 'NONE', #4955, 3.000000000000002665 ) ;
#12712 = CIRCLE ( 'NONE', #1116, 100.0000000000000000 ) ;
#12713 = CARTESIAN_POINT ( 'NONE',  ( -39.30189486418265687, -33.47282819776598473, -8.000000000000000000 ) ) ;
#12714 = CIRCLE ( 'NONE', #3251, 50.00000000000000000 ) ;
#12715 = ORIENTED_EDGE ( 'NONE', *, *, #8008, .T. ) ;
#12716 = CARTESIAN_POINT ( 'NONE',  ( -2.855764796983341736, 2.970025579236414082, -0.09382832055445329555 ) ) ;
#12717 = DIRECTION ( 'NONE',  ( 0.000000000000000000, 0.000000000000000000, 1.000000000000000000 ) ) ;
#12718 = EDGE_CURVE ( 'NONE', #7912, #9770, #14896, .T. ) ;
#12719 = CARTESIAN_POINT ( 'NONE',  ( -92.55687898036933348, -36.52608637591544039, 8.000000000000000000 ) ) ;
#12720 = DIRECTION ( 'NONE',  ( -1.000000000000000000, 0.000000000000000000, 0.000000000000000000 ) ) ;
#12721 = EDGE_LOOP ( 'NONE', ( #3574, #3194, #9610, #5494, #12033, #15009, #6881 ) ) ;
#12722 = CIRCLE ( 'NONE', #11271, 3.000000000000002665 ) ;
#12723 = CIRCLE ( 'NONE', #11014, 95.00000000000001421 ) ;
#12724 = FACE_OUTER_BOUND ( 'NONE', #8409, .T. ) ;
#12725 = FACE_OUTER_BOUND ( 'NONE', #11023, .T. ) ;
#12726 = VECTOR ( 'NONE', #5588, 1000.000000000000000 ) ;
#12727 = EDGE_CURVE ( 'NONE', #1124, #11178, #3010, .T. ) ;
#12728 = CARTESIAN_POINT ( 'NONE',  ( -3.999999999999997335, -1.560351142792952173, -0.2242961665059789167 ) ) ;
#12729 = VERTEX_POINT ( 'NONE', #13244 ) ;
#12730 = ORIENTED_EDGE ( 'NONE', *, *, #3711, .T. ) ;
#12731 = CIRCLE ( 'NONE', #3267, 56.99999999999999289 ) ;
#12732 = ORIENTED_EDGE ( 'NONE', *, *, #13458, .T. ) ;
#12733 = AXIS2_PLACEMENT_3D ( 'NONE', #5443, #10215, #14635 ) ;
#12734 = AXIS2_PLACEMENT_3D ( 'NONE', #8621, #10754, #13267 ) ;
#12735 = CIRCLE ( 'NONE', #5926, 63.00000000000000000 ) ;
#12736 = CARTESIAN_POINT ( 'NONE',  ( 11.62988759722695953, 74.09296836101485439, 17.83282915334323349 ) ) ;
#12737 = VECTOR ( 'NONE', #3511, 1000.000000000000000 ) ;
#12738 = CARTESIAN_POINT ( 'NONE',  ( 5.000000000000004441, 4.249999999999998224, 2.775557561562891351E-14 ) ) ;
#12739 = CARTESIAN_POINT ( 'NONE',  ( 46.63108361037843252, 56.43380494353993271, 10.49999999999999822 ) ) ;
#12740 = FILL_AREA_STYLE ('',( #10225 ) ) ;
#12741 = CYLINDRICAL_SURFACE ( 'NONE', #7163, 56.99999999999999289 ) ;
#12742 = DIRECTION ( 'NONE',  ( 0.000000000000000000, 0.000000000000000000, -1.000000000000000000 ) ) ;
#12743 = VERTEX_POINT ( 'NONE', #2985 ) ;
#12744 = ORIENTED_EDGE ( 'NONE', *, *, #8299, .F. ) ;
#12745 = DIRECTION ( 'NONE',  ( -1.000000000000000000, 0.000000000000000000, 0.000000000000000000 ) ) ;
#12746 = CARTESIAN_POINT ( 'NONE',  ( -30.43807145043581741, 39.66766701456192834, -8.000000000000000000 ) ) ;
#12747 = CIRCLE ( 'NONE', #11042, 52.50000000000000711 ) ;
#12748 = ORIENTED_EDGE ( 'NONE', *, *, #13487, .F. ) ;
#12749 = ORIENTED_EDGE ( 'NONE', *, *, #6528, .T. ) ;
#12750 = DIRECTION ( 'NONE',  ( 0.000000000000000000, 0.000000000000000000, 1.000000000000000000 ) ) ;
#12751 = ADVANCED_FACE ( 'NONE', ( #4128 ), #1994, .F. ) ;
#12752 = ORIENTED_EDGE ( 'NONE', *, *, #9890, .F. ) ;
#12753 = ORIENTED_EDGE ( 'NONE', *, *, #10699, .F. ) ;
#12754 = EDGE_CURVE ( 'NONE', #2530, #4112, #14525, .T. ) ;
#12755 = FACE_OUTER_BOUND ( 'NONE', #14855, .T. ) ;
#12756 = LINE ( 'NONE', #1210, #7062 ) ;
#12757 = EDGE_CURVE ( 'NONE', #8704, #8856, #13677, .T. ) ;
#12758 = CIRCLE ( 'NONE', #6190, 4.000000000000000000 ) ;
#12759 = DIRECTION ( 'NONE',  ( -1.000000000000000000, 1.065814103640150279E-14, 0.000000000000000000 ) ) ;
#12760 = DIRECTION ( 'NONE',  ( 0.000000000000000000, 0.000000000000000000, 1.000000000000000000 ) ) ;
#12761 = ORIENTED_EDGE ( 'NONE', *, *, #7656, .F. ) ;
#12762 = DIRECTION ( 'NONE',  ( -1.000000000000000000, 0.000000000000000000, 0.000000000000000000 ) ) ;
#12763 = VERTEX_POINT ( 'NONE', #11039 ) ;
#12764 = EDGE_CURVE ( 'NONE', #11742, #14537, #1913, .T. ) ;
#12765 = CARTESIAN_POINT ( 'NONE',  ( -4.197393957002299558, 0.4069871074557440682, -3.503767560748926257 ) ) ;
#12766 = ORIENTED_EDGE ( 'NONE', *, *, #11502, .F. ) ;
#12767 = SHAPE_REPRESENTATION ( 'hex flange nut gradea_iso_ISO - 4161 - M5 - N', ( #5108 ), #4118 ) ;
#12768 = EDGE_CURVE ( 'NONE', #4523, #8947, #14161, .T. ) ;
#12769 = FACE_OUTER_BOUND ( 'NONE', #601, .T. ) ;
#12770 = B_SPLINE_CURVE_WITH_KNOTS ( 'NONE', 3,
 ( #3253, #10380, #3475, #13963, #2395, #7874 ),
 .UNSPECIFIED., .F., .F.,
 ( 4, 2, 4 ),
 ( 3.602423855278215334E-18, 0.0002095117440864797216, 0.0004190234881729558111 ),
 .UNSPECIFIED. ) ;
#12771 = CARTESIAN_POINT ( 'NONE',  ( 32.07879498588598466, 95.77069236132479091, 15.33800373393474459 ) ) ;
#12772 = EDGE_CURVE ( 'NONE', #11548, #2568, #6381, .T. ) ;
#12773 = DIRECTION ( 'NONE',  ( -0.000000000000000000, -0.000000000000000000, -1.000000000000000000 ) ) ;
#12774 = CARTESIAN_POINT ( 'NONE',  ( 32.26435573746228158, -42.04772703543541468, -10.50000000000000000 ) ) ;
#12775 = DIRECTION ( 'NONE',  ( 0.000000000000000000, 0.000000000000000000, -1.000000000000000000 ) ) ;
#12776 = DIRECTION ( 'NONE',  ( -0.000000000000000000, -0.000000000000000000, 1.000000000000000000 ) ) ;
#12777 = AXIS2_PLACEMENT_3D ( 'NONE', #7913, #9196, #3360 ) ;
#12778 = DIRECTION ( 'NONE',  ( 1.000000000000000000, 1.749300984178292964E-15, 0.000000000000000000 ) ) ;
#12779 = CONTEXT_DEPENDENT_SHAPE_REPRESENTATION ( #8045, #9843 ) ;
#12780 = DIRECTION ( 'NONE',  ( -1.000000000000000000, 0.000000000000000000, 0.000000000000000000 ) ) ;
#12781 = VERTEX_POINT ( 'NONE', #13385 ) ;
#12782 = DIRECTION ( 'NONE',  ( -1.000000000000000000, 6.308085367188385311E-16, 0.000000000000000000 ) ) ;
#12783 = CARTESIAN_POINT ( 'NONE',  ( 0.000000000000000000, 0.000000000000000000, -13.00000000000000178 ) ) ;
#12784 = DIRECTION ( 'NONE',  ( 0.000000000000000000, 0.000000000000000000, -1.000000000000000000 ) ) ;
#12785 = LINE ( 'NONE', #3529, #5920 ) ;
#12786 = ORIENTED_EDGE ( 'NONE', *, *, #8008, .F. ) ;
#12787 = DIRECTION ( 'NONE',  ( 1.000000000000000000, 0.000000000000000000, 0.000000000000000000 ) ) ;
#12788 = VERTEX_POINT ( 'NONE', #7609 ) ;
#12789 = CARTESIAN_POINT ( 'NONE',  ( -30.00000000000000711, 97.48846085563154418, -31.00000000000000000 ) ) ;
#12790 = PLANE ( 'NONE',  #1514 ) ;
#12791 = ADVANCED_FACE ( 'NONE', ( #4210 ), #9962, .F. ) ;
#12792 = CARTESIAN_POINT ( 'NONE',  ( 26.00011991137315803, 45.91029614918951296, -13.00000000000000178 ) ) ;
#12793 = EDGE_CURVE ( 'NONE', #9152, #11371, #12714, .T. ) ;
#12794 = CARTESIAN_POINT ( 'NONE',  ( 0.000000000000000000, 0.000000000000000000, -13.00000000000000178 ) ) ;
#12795 = EDGE_CURVE ( 'NONE', #10819, #12492, #7607, .T. ) ;
#12796 = VERTEX_POINT ( 'NONE', #14613 ) ;
#12797 = CARTESIAN_POINT ( 'NONE',  ( -32.26435573746199736, 42.04772703543562073, 8.000000000000000000 ) ) ;
#12798 = DIRECTION ( 'NONE',  ( 0.000000000000000000, 0.000000000000000000, 1.000000000000000000 ) ) ;
#12799 = CARTESIAN_POINT ( 'NONE',  ( 0.000000000000000000, 0.000000000000000000, -8.000000000000000000 ) ) ;
#12800 = VERTEX_POINT ( 'NONE', #2906 ) ;
#12801 = EDGE_CURVE ( 'NONE', #5898, #6159, #4473, .T. ) ;
#12802 = VERTEX_POINT ( 'NONE', #2839 ) ;
#12803 = ORIENTED_EDGE ( 'NONE', *, *, #2861, .F. ) ;
#12804 = FACE_OUTER_BOUND ( 'NONE', #6956, .T. ) ;
#12805 = DIRECTION ( 'NONE',  ( 0.000000000000000000, 0.000000000000000000, 1.000000000000000000 ) ) ;
#12806 = EDGE_CURVE ( 'NONE', #490, #11004, #6875, .T. ) ;
#12807 = DIRECTION ( 'NONE',  ( -1.000000000000000000, 0.000000000000000000, 0.000000000000000000 ) ) ;
#12808 =( NAMED_UNIT ( * ) PLANE_ANGLE_UNIT ( ) SI_UNIT ( $, .RADIAN. ) );
#12809 = DIRECTION ( 'NONE',  ( -0.000000000000000000, -0.000000000000000000, 1.000000000000000000 ) ) ;
#12810 = EDGE_LOOP ( 'NONE', ( #9769, #4368, #5510, #1284 ) ) ;
#12811 = DIRECTION ( 'NONE',  ( -0.000000000000000000, -0.000000000000000000, -1.000000000000000000 ) ) ;
#12812 = ORIENTED_EDGE ( 'NONE', *, *, #11567, .T. ) ;
#12813 = VERTEX_POINT ( 'NONE', #6301 ) ;
#12814 = DIRECTION ( 'NONE',  ( -1.000000000000000000, 0.000000000000000000, 0.000000000000000000 ) ) ;
#12815 = DIRECTION ( 'NONE',  ( 1.000000000000000000, 0.000000000000000000, 0.000000000000000000 ) ) ;
#12816 = ORIENTED_EDGE ( 'NONE', *, *, #8016, .T. ) ;
#12817 = ORIENTED_EDGE ( 'NONE', *, *, #12846, .T. ) ;
#12818 = DIRECTION ( 'NONE',  ( -1.000000000000000000, -9.854395544204382819E-14, 0.000000000000000000 ) ) ;
#12819 = CIRCLE ( 'NONE', #6251, 3.000000000000002665 ) ;
#12820 = ORIENTED_EDGE ( 'NONE', *, *, #12301, .F. ) ;
#12821 = CARTESIAN_POINT ( 'NONE',  ( 52.72775723226780542, -7.383907457637739036, -10.50000000000000000 ) ) ;
#12822 = DIRECTION ( 'NONE',  ( 0.000000000000000000, 0.000000000000000000, 1.000000000000000000 ) ) ;
#12823 = CARTESIAN_POINT ( 'NONE',  ( -37.21932736666205699, 89.12622059913296368, -13.00000000000000178 ) ) ;
#12824 = DIRECTION ( 'NONE',  ( -0.000000000000000000, -0.000000000000000000, 1.000000000000000000 ) ) ;
#12825 = CARTESIAN_POINT ( 'NONE',  ( 56.43380494353997534, 12.86891638962136319, 10.49999999999999822 ) ) ;
#12826 = CARTESIAN_POINT ( 'NONE',  ( -91.27544013909712817, 39.61975340586647576, -13.00000000000000178 ) ) ;
#12827 = VERTEX_POINT ( 'NONE', #4059 ) ;
#12828 = DIRECTION ( 'NONE',  ( 0.000000000000000000, 0.000000000000000000, 1.000000000000000000 ) ) ;
#12829 = ORIENTED_EDGE ( 'NONE', *, *, #2162, .F. ) ;
#12830 = EDGE_CURVE ( 'NONE', #13811, #6726, #11743, .T. ) ;
#12831 = CYLINDRICAL_SURFACE ( 'NONE', #1667, 2.649999999999992806 ) ;
#12832 = ORIENTED_EDGE ( 'NONE', *, *, #3139, .T. ) ;
#12833 = CARTESIAN_POINT ( 'NONE',  ( 3.999999999999996447, -2.309401076758518911, -0.5000000000000004441 ) ) ;
#12834 = CIRCLE ( 'NONE', #10645, 100.0000000000000000 ) ;
#12835 = CARTESIAN_POINT ( 'NONE',  ( 27.01438936481372721, 47.21331623427104063, -10.50000000000000000 ) ) ;
#12836 = CARTESIAN_POINT ( 'NONE',  ( 25.00000000000000000, 81.24038404635960831, -16.00000000000000000 ) ) ;
#12837 = FACE_OUTER_BOUND ( 'NONE', #6158, .T. ) ;
#12838 = CARTESIAN_POINT ( 'NONE',  ( -7.830013896347489677, 106.7136370351865935, 19.99999999999999289 ) ) ;
#12839 = FACE_OUTER_BOUND ( 'NONE', #6827, .T. ) ;
#12840 =( GEOMETRIC_REPRESENTATION_CONTEXT ( 3 ) GLOBAL_UNCERTAINTY_ASSIGNED_CONTEXT ( ( #1636 ) ) GLOBAL_UNIT_ASSIGNED_CONTEXT ( ( #12959, #5885, #10825 ) ) REPRESENTATION_CONTEXT ( 'NONE', 'WORKASPACE' ) );
#12841 = DIRECTION ( 'NONE',  ( 1.000000000000000000, 0.000000000000000000, 0.000000000000000000 ) ) ;
#12842 = CONTEXT_DEPENDENT_SHAPE_REPRESENTATION ( #13004, #12539 ) ;
#12843 = LINE ( 'NONE', #14061, #10227 ) ;
#12844 = ORIENTED_EDGE ( 'NONE', *, *, #1854, .T. ) ;
#12845 = ADVANCED_FACE ( 'NONE', ( #5631 ), #10616, .F. ) ;
#12846 = EDGE_CURVE ( 'NONE', #14306, #5756, #5902, .T. ) ;
#12847 = DIRECTION ( 'NONE',  ( 0.000000000000000000, 0.000000000000000000, 1.000000000000000000 ) ) ;
#12848 = DIRECTION ( 'NONE',  ( 0.000000000000000000, 0.000000000000000000, 1.000000000000000000 ) ) ;
#12849 = DIRECTION ( 'NONE',  ( -0.000000000000000000, -0.000000000000000000, 1.000000000000000000 ) ) ;
#12850 = AXIS2_PLACEMENT_3D ( 'NONE', #9547, #216, #6345 ) ;
#12851 = FACE_OUTER_BOUND ( 'NONE', #7739, .T. ) ;
#12852 = EDGE_LOOP ( 'NONE', ( #3844, #2268, #3899, #2199, #2930, #3428, #11851, #13952, #9255, #4484 ) ) ;
#12853 = CIRCLE ( 'NONE', #14802, 56.99999999999999289 ) ;
#12854 = DIRECTION ( 'NONE',  ( 1.000000000000000000, 0.000000000000000000, 0.000000000000000000 ) ) ;
#12855 = VERTEX_POINT ( 'NONE', #2496 ) ;
#12856 = VECTOR ( 'NONE', #3958, 1000.000000000000000 ) ;
#12857 = DIRECTION ( 'NONE',  ( 1.000000000000000000, 0.000000000000000000, 0.000000000000000000 ) ) ;
#12858 = CYLINDRICAL_SURFACE ( 'NONE', #9020, 10.00000000000000178 ) ;
#12859 = DIRECTION ( 'NONE',  ( 0.000000000000000000, 0.000000000000000000, 1.000000000000000000 ) ) ;
#12860 = DIRECTION ( 'NONE',  ( 1.000000000000000000, 0.000000000000000000, 0.000000000000000000 ) ) ;
#12861 = AXIS2_PLACEMENT_3D ( 'NONE', #10406, #5703, #2215 ) ;
#12862 = ORIENTED_EDGE ( 'NONE', *, *, #1074, .F. ) ;
#12863 = CARTESIAN_POINT ( 'NONE',  ( 0.000000000000000000, 0.000000000000000000, 8.000000000000000000 ) ) ;
#12864 = CIRCLE ( 'NONE', #3422, 3.000000000000002665 ) ;
#12865 = DIRECTION ( 'NONE',  ( 1.000000000000000000, 0.000000000000000000, 0.000000000000000000 ) ) ;
#12866 = CIRCLE ( 'NONE', #4393, 50.00000000000000000 ) ;
#12867 = AXIS2_PLACEMENT_3D ( 'NONE', #4489, #14965, #3340 ) ;
#12868 = DIRECTION ( 'NONE',  ( 1.000000000000000000, 0.000000000000000000, 0.000000000000000000 ) ) ;
#12869 = EDGE_LOOP ( 'NONE', ( #9170, #8914, #6572, #6957 ) ) ;
#12870 = EDGE_CURVE ( 'NONE', #4586, #664, #584, .T. ) ;
#12871 = VERTEX_POINT ( 'NONE', #5558 ) ;
#12872 = AXIS2_PLACEMENT_3D ( 'NONE', #1391, #236, #5852 ) ;
#12873 = ORIENTED_EDGE ( 'NONE', *, *, #12665, .T. ) ;
#12874 = AXIS2_PLACEMENT_3D ( 'NONE', #2343, #12678, #9102 ) ;
#12875 = EDGE_CURVE ( 'NONE', #11131, #2090, #213, .T. ) ;
#12876 = DIRECTION ( 'NONE',  ( -1.000000000000000000, 0.000000000000000000, 0.000000000000000000 ) ) ;
#12877 = AXIS2_PLACEMENT_3D ( 'NONE', #9777, #3391, #14866 ) ;
#12878 = FACE_OUTER_BOUND ( 'NONE', #4153, .T. ) ;
#12879 = CIRCLE ( 'NONE', #11428, 0.5000000000000004441 ) ;
#12880 = CYLINDRICAL_SURFACE ( 'NONE', #10014, 95.00000000000001421 ) ;
#12881 = PRESENTATION_STYLE_ASSIGNMENT (( #2556 ) ) ;
#12882 = DIRECTION ( 'NONE',  ( 1.000000000000000000, 0.000000000000000000, 0.000000000000000000 ) ) ;
#12883 = ADVANCED_FACE ( 'NONE', ( #7830 ), #10268, .F. ) ;
#12884 = DIRECTION ( 'NONE',  ( -0.000000000000000000, -0.000000000000000000, -1.000000000000000000 ) ) ;
#12885 = ORIENTED_EDGE ( 'NONE', *, *, #7670, .F. ) ;
#12886 = ORIENTED_EDGE ( 'NONE', *, *, #5380, .T. ) ;
#12887 = EDGE_LOOP ( 'NONE', ( #925, #14639, #7561, #1141, #10234, #2168 ) ) ;
#12888 = CARTESIAN_POINT ( 'NONE',  ( -50.69406879332065330, -13.71740939043347041, -10.50000000000000000 ) ) ;
#12889 = LINE ( 'NONE', #1140, #4804 ) ;
#12890 = CIRCLE ( 'NONE', #14834, 0.5000000000000004441 ) ;
#12891 = VERTEX_POINT ( 'NONE', #67 ) ;
#12892 = ADVANCED_FACE ( 'NONE', ( #7910 ), #13606, .F. ) ;
#12893 = EDGE_CURVE ( 'NONE', #5584, #10382, #4716, .T. ) ;
#12894 = AXIS2_PLACEMENT_3D ( 'NONE', #11122, #717, #7148 ) ;
#12895 = VERTEX_POINT ( 'NONE', #4710 ) ;
#12896 = FACE_OUTER_BOUND ( 'NONE', #661, .T. ) ;
#12897 = VERTEX_POINT ( 'NONE', #2072 ) ;
#12898 = DIRECTION ( 'NONE',  ( 0.9557692240748186796, -0.2941176470588243719, 0.000000000000000000 ) ) ;
#12899 = CARTESIAN_POINT ( 'NONE',  ( -49.00442420935969778, 30.80502811811250297, -13.00000000000000178 ) ) ;
#12900 = AXIS2_PLACEMENT_3D ( 'NONE', #5775, #4577, #3590 ) ;
#12901 = DIRECTION ( 'NONE',  ( 0.000000000000000000, 0.000000000000000000, 1.000000000000000000 ) ) ;
#12902 = DIRECTION ( 'NONE',  ( -1.000000000000000000, 0.000000000000000000, 0.000000000000000000 ) ) ;
#12903 = EDGE_CURVE ( 'NONE', #8404, #1158, #10674, .T. ) ;
#12904 = DIRECTION ( 'NONE',  ( 0.000000000000000000, 0.000000000000000000, 1.000000000000000000 ) ) ;
#12905 = CARTESIAN_POINT ( 'NONE',  ( 33.49014761921571193, 11.74264578624841171, -25.50000000000000355 ) ) ;
#12906 = CIRCLE ( 'NONE', #1265, 53.55662432702593634 ) ;
#12907 = EDGE_LOOP ( 'NONE', ( #1040, #10835, #2286, #12635 ) ) ;
#12908 = CARTESIAN_POINT ( 'NONE',  ( -2.449293598294708880E-16, 38.00000000000000000, -28.00000000000000000 ) ) ;
#12909 = VERTEX_POINT ( 'NONE', #9043 ) ;
#12910 = CIRCLE ( 'NONE', #1756, 56.99999999999999289 ) ;
#12911 = ORIENTED_EDGE ( 'NONE', *, *, #12903, .F. ) ;
#12912 = DIRECTION ( 'NONE',  ( 1.000000000000000000, 0.000000000000000000, 0.000000000000000000 ) ) ;
#12913 = ORIENTED_EDGE ( 'NONE', *, *, #5473, .T. ) ;
#12914 = LINE ( 'NONE', #2505, #9067 ) ;
#12915 = AXIS2_PLACEMENT_3D ( 'NONE', #14009, #7993, #29 ) ;
#12916 = ORIENTED_EDGE ( 'NONE', *, *, #11125, .F. ) ;
#12917 = CARTESIAN_POINT ( 'NONE',  ( 3.861362476283253464, 2.629030857715985992, -3.671615880910370056 ) ) ;
#12918 = CARTESIAN_POINT ( 'NONE',  ( 49.00442420935993226, -30.80502811811213704, -13.00000000000000178 ) ) ;
#12919 = DIRECTION ( 'NONE',  ( -1.000000000000000000, 0.000000000000000000, 0.000000000000000000 ) ) ;
#12920 = CARTESIAN_POINT ( 'NONE',  ( -22.33583958711380646, -30.74264578624812927, -28.00000000000000000 ) ) ;
#12921 = CARTESIAN_POINT ( 'NONE',  ( -4.000000000000369482, 0.8576368993455062428, -3.433240632782570856 ) ) ;
#12922 = AXIS2_PLACEMENT_3D ( 'NONE', #14840, #1101, #2371 ) ;
#12923 = ORIENTED_EDGE ( 'NONE', *, *, #12293, .T. ) ;
#12924 = DIRECTION ( 'NONE',  ( -1.000000000000000000, 0.000000000000000000, 0.000000000000000000 ) ) ;
#12925 = ORIENTED_EDGE ( 'NONE', *, *, #1396, .F. ) ;
#12926 = CARTESIAN_POINT ( 'NONE',  ( -12.33230428938080259, 106.2869539367523544, -16.29453878845857062 ) ) ;
#12927 = DIRECTION ( 'NONE',  ( -0.000000000000000000, -0.000000000000000000, -1.000000000000000000 ) ) ;
#12928 = CIRCLE ( 'NONE', #4450, 102.0000000000000142 ) ;
#12929 = CARTESIAN_POINT ( 'NONE',  ( 5.204748896376250896E-15, 85.00000000000000000, 46.00000000000000000 ) ) ;
#12930 = CARTESIAN_POINT ( 'NONE',  ( -2.000000000000000000, -3.464101615137773926, -3.142992957459240344 ) ) ;
#12931 = AXIS2_PLACEMENT_3D ( 'NONE', #2204, #6820, #8950 ) ;
#12932 = ORIENTED_EDGE ( 'NONE', *, *, #800, .F. ) ;
#12933 = EDGE_CURVE ( 'NONE', #1331, #1743, #6637, .T. ) ;
#12934 = DIRECTION ( 'NONE',  ( -1.000000000000000000, 0.000000000000000000, 0.000000000000000000 ) ) ;
#12935 = EDGE_LOOP ( 'NONE', ( #8216, #5568 ) ) ;
#12936 = ADVANCED_FACE ( 'NONE', ( #3213, #942 ), #10186, .T. ) ;
#12937 = VERTEX_POINT ( 'NONE', #3290 ) ;
#12938 = CARTESIAN_POINT ( 'NONE',  ( 33.49014761921571903, 11.74264578624841171, -28.00000000000000000 ) ) ;
#12939 = ADVANCED_FACE ( 'NONE', ( #12139 ), #3800, .F. ) ;
#12940 = CARTESIAN_POINT ( 'NONE',  ( -3.492805317593278058, 46.55633131742322917, -10.50000000000000000 ) ) ;
#12941 = EDGE_CURVE ( 'NONE', #3450, #9063, #12069, .T. ) ;
#12942 = CARTESIAN_POINT ( 'NONE',  ( -2.449293598294700991E-16, 97.00000000000000000, -13.00000000000000178 ) ) ;
#12943 = CARTESIAN_POINT ( 'NONE',  ( 0.000000000000000000, 0.000000000000000000, -43.49999999999998579 ) ) ;
#12944 = ORIENTED_EDGE ( 'NONE', *, *, #6310, .T. ) ;
#12945 = CIRCLE ( 'NONE', #14889, 56.99999999999999289 ) ;
#12946 = CARTESIAN_POINT ( 'NONE',  ( -26.49999999999971578, -45.89934640057541060, 10.49999999999999822 ) ) ;
#12947 = ADVANCED_FACE ( 'NONE', ( #298 ), #1437, .F. ) ;
#12948 = LINE ( 'NONE', #2541, #9549 ) ;
#12949 = DIRECTION ( 'NONE',  ( -0.000000000000000000, -0.000000000000000000, -1.000000000000000000 ) ) ;
#12950 = AXIS2_PLACEMENT_3D ( 'NONE', #1222, #9262, #14975 ) ;
#12951 = ORIENTED_EDGE ( 'NONE', *, *, #4068, .F. ) ;
#12952 = ORIENTED_EDGE ( 'NONE', *, *, #1125, .F. ) ;
#12953 = EDGE_LOOP ( 'NONE', ( #3110, #12644, #196, #2860, #3215 ) ) ;
#12954 = EDGE_CURVE ( 'NONE', #8947, #1277, #14094, .T. ) ;
#12955 = CARTESIAN_POINT ( 'NONE',  ( 10.55213320575002101, 106.4787665061024597, 18.97395805252363843 ) ) ;
#12956 = DIRECTION ( 'NONE',  ( 1.000000000000000000, 0.000000000000000000, 0.000000000000000000 ) ) ;
#12957 = DIRECTION ( 'NONE',  ( -0.000000000000000000, -0.000000000000000000, 1.000000000000000000 ) ) ;
#12958 = AXIS2_PLACEMENT_3D ( 'NONE', #2301, #6986, #13850 ) ;
#12959 =( LENGTH_UNIT ( ) NAMED_UNIT ( * ) SI_UNIT ( .MILLI., .METRE. ) );
#12960 = DIRECTION ( 'NONE',  ( 0.000000000000000000, 0.000000000000000000, -1.000000000000000000 ) ) ;
#12961 = TOROIDAL_SURFACE ( 'NONE', #11274, 17.00000000000000000, 5.000000000000000000 ) ;
#12962 = ORIENTED_EDGE ( 'NONE', *, *, #11727, .F. ) ;
#12963 = VERTEX_POINT ( 'NONE', #2870 ) ;
#12964 = LINE ( 'NONE', #1422, #7385 ) ;
#12965 = CARTESIAN_POINT ( 'NONE',  ( 69.20695371924547601, 57.06275842387054098, -13.00000000000000178 ) ) ;
#12966 = DIRECTION ( 'NONE',  ( 0.000000000000000000, 0.000000000000000000, -1.000000000000000000 ) ) ;
#12967 = ORIENTED_EDGE ( 'NONE', *, *, #7656, .T. ) ;
#12968 = AXIS2_PLACEMENT_3D ( 'NONE', #13854, #11508, #3449 ) ;
#12969 = ORIENTED_EDGE ( 'NONE', *, *, #13980, .F. ) ;
#12970 = CARTESIAN_POINT ( 'NONE',  ( 57.06275842387049835, -9.706953719245678514, -10.50000000000000000 ) ) ;
#12971 = VECTOR ( 'NONE', #2775, 1000.000000000000000 ) ;
#12972 = AXIS2_PLACEMENT_3D ( 'NONE', #5044, #13024, #14236 ) ;
#12973 = CIRCLE ( 'NONE', #6406, 3.000000000000002665 ) ;
#12974 = VERTEX_POINT ( 'NONE', #1591 ) ;
#12975 = CARTESIAN_POINT ( 'NONE',  ( 33.47282819776613394, -39.30189486418255740, 8.000000000000000000 ) ) ;
#12976 = CARTESIAN_POINT ( 'NONE',  ( 89.12622059913255157, 37.21932736666302333, 10.49999999999999822 ) ) ;
#12977 = CARTESIAN_POINT ( 'NONE',  ( -45.83364790889027773, 29.49928053175948506, 8.000000000000000000 ) ) ;
#12979 = ORIENTED_EDGE ( 'NONE', *, *, #2586, .T. ) ;
#12978 = ADVANCED_FACE ( 'NONE', ( #14335 ), #8482, .F. ) ;
#12980 = CIRCLE ( 'NONE', #14428, 22.00000000000001421 ) ;
#12981 = CARTESIAN_POINT ( 'NONE',  ( -12.05075418994416125, 74.02560756970278533, -17.09116503294089640 ) ) ;
#12982 = DIRECTION ( 'NONE',  ( -0.000000000000000000, -0.000000000000000000, 1.000000000000000000 ) ) ;
#12983 = EDGE_CURVE ( 'NONE', #1155, #2510, #4640, .T. ) ;
#12984 = ORIENTED_EDGE ( 'NONE', *, *, #2258, .T. ) ;
#12985 = AXIS2_PLACEMENT_3D ( 'NONE', #4224, #2998, #12273 ) ;
#12986 = AXIS2_PLACEMENT_3D ( 'NONE', #11269, #6693, #3218 ) ;
#12987 = CARTESIAN_POINT ( 'NONE',  ( -68.58935777509427112, 68.58935777509594800, -13.00000000000000178 ) ) ;
#12988 = CIRCLE ( 'NONE', #4507, 60.50000000000000711 ) ;
#12989 = EDGE_CURVE ( 'NONE', #6551, #13229, #4936, .T. ) ;
#12990 = ORIENTED_EDGE ( 'NONE', *, *, #8625, .T. ) ;
#12991 = ORIENTED_EDGE ( 'NONE', *, *, #6230, .T. ) ;
#12992 = DIRECTION ( 'NONE',  ( -1.000000000000000000, 0.000000000000000000, 0.000000000000000000 ) ) ;
#12993 = CIRCLE ( 'NONE', #6916, 5.000000000000001776 ) ;
#12994 = EDGE_CURVE ( 'NONE', #6180, #10678, #9706, .T. ) ;
#12995 = AXIS2_PLACEMENT_3D ( 'NONE', #2733, #1521, #7349 ) ;
#12996 = DIRECTION ( 'NONE',  ( 0.000000000000000000, 0.000000000000000000, -1.000000000000000000 ) ) ;
#12997 = CARTESIAN_POINT ( 'NONE',  ( 32.45028783375101966, 101.9412720646926118, -14.06019896931748647 ) ) ;
#12998 = FACE_OUTER_BOUND ( 'NONE', #4694, .T. ) ;
#12999 = FACE_OUTER_BOUND ( 'NONE', #13457, .T. ) ;
#13000 = DIRECTION ( 'NONE',  ( 0.000000000000000000, 0.000000000000000000, -1.000000000000000000 ) ) ;
#13001 = DIRECTION ( 'NONE',  ( 0.000000000000000000, 0.000000000000000000, 1.000000000000000000 ) ) ;
#13002 = ADVANCED_FACE ( 'NONE', ( #13130 ), #14414, .T. ) ;
#13003 = VERTEX_POINT ( 'NONE', #12002 ) ;
#13004 =( REPRESENTATION_RELATIONSHIP ('NONE','NONE', #12187, #8006 ) REPRESENTATION_RELATIONSHIP_WITH_TRANSFORMATION ( #8137 )SHAPE_REPRESENTATION_RELATIONSHIP( ) );
#13005 = AXIS2_PLACEMENT_3D ( 'NONE', #5580, #9148, #1181 ) ;
#13006 = EDGE_LOOP ( 'NONE', ( #3557, #5864, #9161, #7741, #4535, #6641 ) ) ;
#13007 = CARTESIAN_POINT ( 'NONE',  ( 1.828356344711641102, 3.563200125723179568, 1.655949411882156916E-16 ) ) ;
#13008 = DIRECTION ( 'NONE',  ( 0.000000000000000000, 0.000000000000000000, 1.000000000000000000 ) ) ;
#13009 = DIRECTION ( 'NONE',  ( 0.000000000000000000, 0.000000000000000000, -1.000000000000000000 ) ) ;
#13010 = DIRECTION ( 'NONE',  ( 0.8660254037844374864, -0.5000000000000018874, 0.000000000000000000 ) ) ;
#13011 = VERTEX_POINT ( 'NONE', #6204 ) ;
#13012 = CIRCLE ( 'NONE', #165, 0.5000000000000004441 ) ;
#13013 = CARTESIAN_POINT ( 'NONE',  ( 32.06294366074496338, -42.50536573064421475, -10.50000000000000000 ) ) ;
#13014 = ORIENTED_EDGE ( 'NONE', *, *, #14273, .T. ) ;
#13015 = CARTESIAN_POINT ( 'NONE',  ( 69.16568774265594755, -71.53347797788796925, -8.000000000000000000 ) ) ;
#13016 = CARTESIAN_POINT ( 'NONE',  ( 0.000000000000000000, 0.000000000000000000, 8.000000000000000000 ) ) ;
#13017 = DIRECTION ( 'NONE',  ( 1.000000000000000000, -3.498601968356585929E-15, 0.000000000000000000 ) ) ;
#13018 = CARTESIAN_POINT ( 'NONE',  ( 0.000000000000000000, 0.000000000000000000, 8.000000000000000000 ) ) ;
#13019 = CIRCLE ( 'NONE', #6450, 0.5000000000000004441 ) ;
#13020 = VERTEX_POINT ( 'NONE', #10843 ) ;
#13021 = VERTEX_POINT ( 'NONE', #6341 ) ;
#13022 = AXIS2_PLACEMENT_3D ( 'NONE', #11170, #462, #9866 ) ;
#13023 = DIRECTION ( 'NONE',  ( 1.000000000000000000, 0.000000000000000000, -0.000000000000000000 ) ) ;
#13024 = DIRECTION ( 'NONE',  ( 0.000000000000000000, 0.000000000000000000, -1.000000000000000000 ) ) ;
#13025 = DIRECTION ( 'NONE',  ( 0.000000000000000000, -1.000000000000000000, -0.000000000000000000 ) ) ;
#13026 = EDGE_CURVE ( 'NONE', #1392, #6713, #13053, .T. ) ;
#13027 = EDGE_CURVE ( 'NONE', #1277, #9852, #2446, .T. ) ;
#13028 = ORIENTED_EDGE ( 'NONE', *, *, #1289, .F. ) ;
#13029 = ORIENTED_EDGE ( 'NONE', *, *, #10429, .F. ) ;
#13030 = DIRECTION ( 'NONE',  ( 0.000000000000000000, 0.000000000000000000, 1.000000000000000000 ) ) ;
#13031 = ORIENTED_EDGE ( 'NONE', *, *, #10929, .F. ) ;
#13032 = CARTESIAN_POINT ( 'NONE',  ( 5.204748896376250896E-15, 85.00000000000000000, 31.00000000000000000 ) ) ;
#13033 = CARTESIAN_POINT ( 'NONE',  ( 29.49928053175901610, 45.83364790889059037, -8.000000000000000000 ) ) ;
#13034 = CARTESIAN_POINT ( 'NONE',  ( -68.58935777509427112, 68.58935777509594800, 10.49999999999999822 ) ) ;
#13035 = FILL_AREA_STYLE_COLOUR ( '', #2895 ) ;
#13036 = CARTESIAN_POINT ( 'NONE',  ( -31.56034153936678521, 95.94279256428042402, -14.97248702055886582 ) ) ;
#13037 = ORIENTED_EDGE ( 'NONE', *, *, #404, .F. ) ;
#13038 = EDGE_LOOP ( 'NONE', ( #3095, #13198, #14099, #3257 ) ) ;
#13039 = CARTESIAN_POINT ( 'NONE',  ( -33.48561063518626923, 47.21331623427104063, -13.00000000000000178 ) ) ;
#13040 = PLANE ( 'NONE',  #11354 ) ;
#13041 = CARTESIAN_POINT ( 'NONE',  ( 2.500000000000000444, 0.000000000000000000, -25.03750572909317285 ) ) ;
#13042 = EDGE_CURVE ( 'NONE', #5870, #12645, #2695, .T. ) ;
#13044 = ORIENTED_EDGE ( 'NONE', *, *, #11143, .T. ) ;
#13043 = EDGE_CURVE ( 'NONE', #5260, #3630, #599, .T. ) ;
#13045 = AXIS2_PLACEMENT_3D ( 'NONE', #3256, #3330, #1060 ) ;
#13046 = ORIENTED_EDGE ( 'NONE', *, *, #2359, .T. ) ;
#13047 = CARTESIAN_POINT ( 'NONE',  ( -30.43807145043584583, 39.66766701456190702, 8.000000000000000000 ) ) ;
#13048 = ORIENTED_EDGE ( 'NONE', *, *, #6810, .T. ) ;
#13049 = CARTESIAN_POINT ( 'NONE',  ( -38.26834323650965786, -92.38795325112840828, 8.000000000000000000 ) ) ;
#13050 = CARTESIAN_POINT ( 'NONE',  ( -1.674280531759317459, 94.51066581171355097, -8.000000000000000000 ) ) ;
#13051 = FACE_OUTER_BOUND ( 'NONE', #14942, .T. ) ;
#13052 = ORIENTED_EDGE ( 'NONE', *, *, #5067, .T. ) ;
#13053 = LINE ( 'NONE', #8634, #9233 ) ;
#13054 = CIRCLE ( 'NONE', #9883, 50.00000000000000000 ) ;
#13055 = DIRECTION ( 'NONE',  ( 1.000000000000000000, 0.000000000000000000, 0.000000000000000000 ) ) ;
#13056 = ORIENTED_EDGE ( 'NONE', *, *, #1435, .F. ) ;
#13057 = DIRECTION ( 'NONE',  ( 0.000000000000000000, 0.000000000000000000, 1.000000000000000000 ) ) ;
#13058 = VERTEX_POINT ( 'NONE', #9686 ) ;
#13059 = VERTEX_POINT ( 'NONE', #5154 ) ;
#13060 =( NAMED_UNIT ( * ) PLANE_ANGLE_UNIT ( ) SI_UNIT ( $, .RADIAN. ) );
#13061 = EDGE_CURVE ( 'NONE', #2546, #8947, #4093, .T. ) ;
#13062 = DIRECTION ( 'NONE',  ( 0.000000000000000000, 0.000000000000000000, 1.000000000000000000 ) ) ;
#13063 = ADVANCED_FACE ( 'NONE', ( #8557 ), #9544, .T. ) ;
#13064 = ORIENTED_EDGE ( 'NONE', *, *, #6612, .T. ) ;
#13065 = DIRECTION ( 'NONE',  ( 0.000000000000000000, 0.000000000000000000, 1.000000000000000000 ) ) ;
#13066 = EDGE_CURVE ( 'NONE', #7929, #11386, #10446, .T. ) ;
#13067 = CARTESIAN_POINT ( 'NONE',  ( 2.500000000000002220, 0.000000000000000000, 0.000000000000000000 ) ) ;
#13068 = CARTESIAN_POINT ( 'NONE',  ( 40.12029293941316155, -89.61631465359504034, -8.000000000000000000 ) ) ;
#13069 = DIRECTION ( 'NONE',  ( -0.000000000000000000, -0.000000000000000000, -1.000000000000000000 ) ) ;
#13070 = CARTESIAN_POINT ( 'NONE',  ( 15.88467684210547226, -49.11971303961683333, 8.000000000000000000 ) ) ;
#13071 = ORIENTED_EDGE ( 'NONE', *, *, #2233, .T. ) ;
#13072 = ADVANCED_FACE ( 'NONE', ( #13499 ), #3252, .T. ) ;
#13073 = CARTESIAN_POINT ( 'NONE',  ( -45.89934640057513349, 26.50000000000019540, 8.000000000000000000 ) ) ;
#13074 = ORIENTED_EDGE ( 'NONE', *, *, #792, .F. ) ;
#13075 = FACE_OUTER_BOUND ( 'NONE', #8311, .T. ) ;
#13076 = CIRCLE ( 'NONE', #7969, 0.5000000000000004441 ) ;
#13077 = CARTESIAN_POINT ( 'NONE',  ( -37.02125851216292318, 90.10640870805768543, -10.50000000000000000 ) ) ;
#13078 = DIRECTION ( 'NONE',  ( -1.000000000000000000, 0.000000000000000000, 0.000000000000000000 ) ) ;
#13079 = ADVANCED_FACE ( 'NONE', ( #830 ), #4397, .T. ) ;
#13080 = CARTESIAN_POINT ( 'NONE',  ( 31.47058823529413729, 102.2673069760056563, 10.99999999999999645 ) ) ;
#13081 = EDGE_CURVE ( 'NONE', #6653, #8389, #8502, .T. ) ;
#13082 = ORIENTED_EDGE ( 'NONE', *, *, #4723, .F. ) ;
#13083 = DIRECTION ( 'NONE',  ( 1.000000000000000000, 0.000000000000000000, 0.000000000000000000 ) ) ;
#13084 = AXIS2_PLACEMENT_3D ( 'NONE', #6321, #9899, #14543 ) ;
#13085 = EDGE_LOOP ( 'NONE', ( #2865, #11609, #7036, #11191, #14560, #11448, #3546, #13265, #10458 ) ) ;
#13086 = ORIENTED_EDGE ( 'NONE', *, *, #7070, .T. ) ;
#13087 = FACE_OUTER_BOUND ( 'NONE', #7480, .T. ) ;
#13088 = DIRECTION ( 'NONE',  ( 0.2941176470588238168, -0.9557692240748187906, 0.000000000000000000 ) ) ;
#13089 = AXIS2_PLACEMENT_3D ( 'NONE', #7424, #7343, #1513 ) ;
#13090 = CARTESIAN_POINT ( 'NONE',  ( -48.19406879332065330, -13.71740939043347041, -8.000000000000000000 ) ) ;
#13091 = DIRECTION ( 'NONE',  ( 1.000000000000000000, 0.000000000000000000, 0.000000000000000000 ) ) ;
#13092 = VERTEX_POINT ( 'NONE', #14793 ) ;
#13093 = DIRECTION ( 'NONE',  ( -1.000000000000000000, 6.927231897346039366E-14, 0.000000000000000000 ) ) ;
#13094 = DIRECTION ( 'NONE',  ( 1.000000000000000000, 0.000000000000000000, 0.000000000000000000 ) ) ;
#13095 = DIRECTION ( 'NONE',  ( -1.000000000000000000, 0.000000000000000000, 0.000000000000000000 ) ) ;
#13096 = AXIS2_PLACEMENT_3D ( 'NONE', #833, #6430, #6496 ) ;
#13097 = CARTESIAN_POINT ( 'NONE',  ( -12.39897948556635754, 100.2360479454198696, 16.00000000000000000 ) ) ;
#13098 = CIRCLE ( 'NONE', #13827, 4.250000000000000000 ) ;
#13099 = VECTOR ( 'NONE', #12308, 1000.000000000000000 ) ;
#13100 = ORIENTED_EDGE ( 'NONE', *, *, #10567, .F. ) ;
#13101 = DIRECTION ( 'NONE',  ( 0.000000000000000000, 0.000000000000000000, 1.000000000000000000 ) ) ;
#13102 = ORIENTED_EDGE ( 'NONE', *, *, #9961, .T. ) ;
#13103 = CYLINDRICAL_SURFACE ( 'NONE', #13699, 5.000000000000000888 ) ;
#13104 = VERTEX_POINT ( 'NONE', #7873 ) ;
#13105 = VECTOR ( 'NONE', #6683, 1000.000000000000000 ) ;
#13106 = DIRECTION ( 'NONE',  ( -0.000000000000000000, -0.000000000000000000, -1.000000000000000000 ) ) ;
#13107 = CARTESIAN_POINT ( 'NONE',  ( 1.287237434361648170, 3.875615274277123934, -3.430618716626443021 ) ) ;
#13108 = CARTESIAN_POINT ( 'NONE',  ( -29.70588235294118107, 96.53269163155674448, -11.33021710499463630 ) ) ;
#13109 = AXIS2_PLACEMENT_3D ( 'NONE', #6278, #535, #9561 ) ;
#13110 = ORIENTED_EDGE ( 'NONE', *, *, #13690, .F. ) ;
#13111 = EDGE_LOOP ( 'NONE', ( #14478, #3685, #9800, #8547, #5485, #14751, #12543, #5995, #11380, #11360 ) ) ;
#13112 = PRESENTATION_LAYER_ASSIGNMENT (  '', '', ( #4862 ) ) ;
#13113 = CARTESIAN_POINT ( 'NONE',  ( -12.86891638962156215, 56.43380494353993271, -10.50000000000000000 ) ) ;
#13114 = DIRECTION ( 'NONE',  ( -1.000000000000000000, 0.000000000000000000, 0.000000000000000000 ) ) ;
#13115 = DIRECTION ( 'NONE',  ( -0.000000000000000000, -0.000000000000000000, 1.000000000000000000 ) ) ;
#13116 = VERTEX_POINT ( 'NONE', #14728 ) ;
#13117 = AXIS2_PLACEMENT_3D ( 'NONE', #10860, #2595, #13149 ) ;
#13118 = VECTOR ( 'NONE', #7186, 1000.000000000000000 ) ;
#13119 = VERTEX_POINT ( 'NONE', #3103 ) ;
#13120 = CARTESIAN_POINT ( 'NONE',  ( 9.706953719245472456, 57.06275842387054098, -13.00000000000000178 ) ) ;
#13121 = CIRCLE ( 'NONE', #8500, 53.55662432702593634 ) ;
#13122 = VERTEX_POINT ( 'NONE', #13565 ) ;
#13123 = AXIS2_PLACEMENT_3D ( 'NONE', #6127, #11076, #5454 ) ;
#13124 = DIRECTION ( 'NONE',  ( 0.000000000000000000, 0.000000000000000000, 1.000000000000000000 ) ) ;
#13125 = EDGE_CURVE ( 'NONE', #4787, #14448, #1010, .T. ) ;
#13126 = CARTESIAN_POINT ( 'NONE',  ( 0.5469614295412751348, -4.303013824935497667, -3.535263753543608001 ) ) ;
#13127 = EDGE_CURVE ( 'NONE', #6408, #5997, #4878, .T. ) ;
#13128 = EDGE_CURVE ( 'NONE', #3028, #7285, #3030, .T. ) ;
#13129 = ORIENTED_EDGE ( 'NONE', *, *, #4818, .T. ) ;
#13131 = CIRCLE ( 'NONE', #14103, 59.50000000000000000 ) ;
#13130 = FACE_OUTER_BOUND ( 'NONE', #5361, .T. ) ;
#13132 = DIRECTION ( 'NONE',  ( -0.000000000000000000, -0.000000000000000000, -1.000000000000000000 ) ) ;
#13133 = VERTEX_POINT ( 'NONE', #12441 ) ;
#13134 = CIRCLE ( 'NONE', #33, 3.000000000000002665 ) ;
#13135 = DIRECTION ( 'NONE',  ( -0.000000000000000000, -0.000000000000000000, 1.000000000000000000 ) ) ;
#13136 = CIRCLE ( 'NONE', #3684, 3.000000000000002665 ) ;
#13137 = VERTEX_POINT ( 'NONE', #11147 ) ;
#13138 = ORIENTED_EDGE ( 'NONE', *, *, #2793, .F. ) ;
#13139 = CARTESIAN_POINT ( 'NONE',  ( 0.000000000000000000, 0.000000000000000000, 23.50000000000000355 ) ) ;
#13140 = VECTOR ( 'NONE', #5493, 1000.000000000000000 ) ;
#13141 = VERTEX_POINT ( 'NONE', #5527 ) ;
#13142 = CARTESIAN_POINT ( 'NONE',  ( -2.649999999999987921, 38.00000000000000000, -25.50000000000000355 ) ) ;
#13143 = CIRCLE ( 'NONE', #6579, 3.000000000000002665 ) ;
#13144 = DIRECTION ( 'NONE',  ( 0.000000000000000000, 0.000000000000000000, 1.000000000000000000 ) ) ;
#13145 = FACE_OUTER_BOUND ( 'NONE', #14717, .T. ) ;
#13146 = CYLINDRICAL_SURFACE ( 'NONE', #5095, 14.00000000000000000 ) ;
#13147 = DIRECTION ( 'NONE',  ( 1.000000000000000000, 0.000000000000000000, 0.000000000000000000 ) ) ;
#13148 = ORIENTED_EDGE ( 'NONE', *, *, #14281, .F. ) ;
#13149 = DIRECTION ( 'NONE',  ( -1.000000000000000000, 0.000000000000000000, 0.000000000000000000 ) ) ;
#13150 = CIRCLE ( 'NONE', #8012, 75.00000000000001421 ) ;
#13151 = ORIENTED_EDGE ( 'NONE', *, *, #7025, .T. ) ;
#13152 = EDGE_CURVE ( 'NONE', #9152, #5654, #2035, .T. ) ;
#13153 = CARTESIAN_POINT ( 'NONE',  ( -11.47554877443044141, 106.3830115231064184, -18.04988257186027667 ) ) ;
#13154 = CARTESIAN_POINT ( 'NONE',  ( -68.58935777509427112, 68.58935777509594800, 8.000000000000000000 ) ) ;
#13155 = CIRCLE ( 'NONE', #7569, 60.50000000000000000 ) ;
#13156 = DIRECTION ( 'NONE',  ( -1.000000000000000000, 0.000000000000000000, -0.000000000000000000 ) ) ;
#13157 = CYLINDRICAL_SURFACE ( 'NONE', #13673, 3.000000000000002665 ) ;
#13158 = ORIENTED_EDGE ( 'NONE', *, *, #13546, .T. ) ;
#13159 = CARTESIAN_POINT ( 'NONE',  ( -19.68583958711381143, -30.74264578624812927, -28.00000000000000000 ) ) ;
#13160 = VERTEX_POINT ( 'NONE', #12519 ) ;
#13161 = CIRCLE ( 'NONE', #6339, 60.50000000000000000 ) ;
#13162 = DIRECTION ( 'NONE',  ( -1.000000000000000000, 0.000000000000000000, 0.000000000000000000 ) ) ;
#13163 = DIRECTION ( 'NONE',  ( -0.000000000000000000, -0.000000000000000000, -1.000000000000000000 ) ) ;
#13164 = CARTESIAN_POINT ( 'NONE',  ( -33.32958405265415536, 101.6044047647130384, -14.99207720203048844 ) ) ;
#13165 = AXIS2_PLACEMENT_3D ( 'NONE', #11187, #786, #7750 ) ;
#13166 = CARTESIAN_POINT ( 'NONE',  ( 68.58935777509475429, -68.58935777509547904, 10.49999999999999822 ) ) ;
#13167 = CARTESIAN_POINT ( 'NONE',  ( -26.49999999999971578, -45.89934640057541060, 8.000000000000000000 ) ) ;
#13168 = EDGE_CURVE ( 'NONE', #10287, #11546, #264, .T. ) ;
#13169 = ORIENTED_EDGE ( 'NONE', *, *, #10429, .T. ) ;
#13170 = ORIENTED_EDGE ( 'NONE', *, *, #5632, .T. ) ;
#13171 = ADVANCED_FACE ( 'NONE', ( #13651, #4250, #7652, #11229, #2109, #7798, #8786 ), #12216, .F. ) ;
#13172 = CARTESIAN_POINT ( 'NONE',  ( -32.26435573746199736, 42.04772703543562073, -8.000000000000000000 ) ) ;
#13173 = CARTESIAN_POINT ( 'NONE',  ( -86.67575032682103142, -37.71449950291016506, -13.00000000000000178 ) ) ;
#13174 = CIRCLE ( 'NONE', #4443, 2.100000000000000089 ) ;
#13175 = DIRECTION ( 'NONE',  ( -1.000000000000000000, 0.000000000000000000, 0.000000000000000000 ) ) ;
#13176 = AXIS2_PLACEMENT_3D ( 'NONE', #543, #8507, #13232 ) ;
#13177 = PRODUCT_DEFINITION_CONTEXT ( 'detailed design', #11651, 'design' ) ;
#13178 = VERTEX_POINT ( 'NONE', #6651 ) ;
#13179 = ADVANCED_FACE ( 'NONE', ( #11308 ), #910, .F. ) ;
#13180 = CARTESIAN_POINT ( 'NONE',  ( -19.68583958711381143, -30.74264578624812927, -25.50000000000000355 ) ) ;
#13181 = EDGE_LOOP ( 'NONE', ( #8320, #13138, #12885, #14299, #4768, #742 ) ) ;
#13182 = CARTESIAN_POINT ( 'NONE',  ( -42.00000000000000000, 81.24038404635962252, -31.00000000000000000 ) ) ;
#13183 = AXIS2_PLACEMENT_3D ( 'NONE', #4043, #6363, #11018 ) ;
#13184 = DIRECTION ( 'NONE',  ( 0.000000000000000000, 0.000000000000000000, 1.000000000000000000 ) ) ;
#13185 = DIRECTION ( 'NONE',  ( 1.000000000000000000, 0.000000000000000000, 0.000000000000000000 ) ) ;
#13186 = APPLICATION_PROTOCOL_DEFINITION ( 'draft international standard', 'automotive_design', 1998, #6085 ) ;
#13187 = CARTESIAN_POINT ( 'NONE',  ( -34.44830544488820578, 94.94374256356073261, -16.00000000000000000 ) ) ;
#13188 = ORIENTED_EDGE ( 'NONE', *, *, #11021, .F. ) ;
#13189 = EDGE_CURVE ( 'NONE', #14956, #11572, #1638, .T. ) ;
#13190 = AXIS2_PLACEMENT_3D ( 'NONE', #2017, #8847, #1870 ) ;
#13191 = DIRECTION ( 'NONE',  ( 0.000000000000000000, 0.000000000000000000, 1.000000000000000000 ) ) ;
#13192 = DIRECTION ( 'NONE',  ( -0.000000000000000000, -0.000000000000000000, 1.000000000000000000 ) ) ;
#13193 = VECTOR ( 'NONE', #12641, 999.9999999999998863 ) ;
#13194 = LINE ( 'NONE', #3790, #8080 ) ;
#13195 = ORIENTED_EDGE ( 'NONE', *, *, #700, .T. ) ;
#13196 = ORIENTED_EDGE ( 'NONE', *, *, #4028, .T. ) ;
#13197 = DIRECTION ( 'NONE',  ( -1.000000000000000000, -1.332267629550187849E-14, 0.000000000000000000 ) ) ;
#13198 = ORIENTED_EDGE ( 'NONE', *, *, #6845, .T. ) ;
#13199 =( REPRESENTATION_RELATIONSHIP ('NONE','NONE', #12187, #12767 ) REPRESENTATION_RELATIONSHIP_WITH_TRANSFORMATION ( #3960 )SHAPE_REPRESENTATION_RELATIONSHIP( ) );
#13200 = TOROIDAL_SURFACE ( 'NONE', #13935, 102.0000000000000142, 5.000000000000000000 ) ;
#13202 = DIRECTION ( 'NONE',  ( -0.000000000000000000, -0.000000000000000000, 1.000000000000000000 ) ) ;
#13201 = CIRCLE ( 'NONE', #3502, 3.000000000000002665 ) ;
#13203 = AXIS2_PLACEMENT_3D ( 'NONE', #1775, #4290, #14374 ) ;
#13204 = DIRECTION ( 'NONE',  ( 0.000000000000000000, 0.000000000000000000, 1.000000000000000000 ) ) ;
#13205 = CYLINDRICAL_SURFACE ( 'NONE', #3172, 56.99999999999999289 ) ;
#13206 = ORIENTED_EDGE ( 'NONE', *, *, #5474, .F. ) ;
#13207 = CARTESIAN_POINT ( 'NONE',  ( 2.500000000000002220, 2.357898499370430834, -6.938893903907228378E-15 ) ) ;
#13208 = DIRECTION ( 'NONE',  ( -1.000000000000000000, 0.000000000000000000, 0.000000000000000000 ) ) ;
#13209 = ORIENTED_EDGE ( 'NONE', *, *, #13306, .F. ) ;
#13210 = DIRECTION ( 'NONE',  ( 0.000000000000000000, 0.000000000000000000, 1.000000000000000000 ) ) ;
#13211 = AXIS2_PLACEMENT_3D ( 'NONE', #4840, #14257, #7250 ) ;
#13212 = CIRCLE ( 'NONE', #6644, 22.00000000000001421 ) ;
#13213 = AXIS2_PLACEMENT_3D ( 'NONE', #12651, #8227, #2247 ) ;
#13214 = ORIENTED_EDGE ( 'NONE', *, *, #5698, .F. ) ;
#13215 = AXIS2_PLACEMENT_3D ( 'NONE', #7107, #293, #9842 ) ;
#13216 = ORIENTED_EDGE ( 'NONE', *, *, #3078, .T. ) ;
#13217 = DIRECTION ( 'NONE',  ( 0.000000000000000000, 0.000000000000000000, -1.000000000000000000 ) ) ;
#13218 = ADVANCED_FACE ( 'NONE', ( #7315 ), #3841, .T. ) ;
#13219 = ADVANCED_FACE ( 'NONE', ( #4984 ), #6243, .T. ) ;
#13220 = FACE_OUTER_BOUND ( 'NONE', #5713, .T. ) ;
#13221 = AXIS2_PLACEMENT_3D ( 'NONE', #14746, #12466, #3278 ) ;
#13222 = DIRECTION ( 'NONE',  ( 1.000000000000000000, 0.000000000000000000, 0.000000000000000000 ) ) ;
#13223 = DIRECTION ( 'NONE',  ( 1.000000000000000000, 0.000000000000000000, 0.000000000000000000 ) ) ;
#13224 = CARTESIAN_POINT ( 'NONE',  ( -70.71067811865385977, 70.71067811865565034, -8.000000000000000000 ) ) ;
#13225 = EDGE_CURVE ( 'NONE', #9910, #2855, #421, .T. ) ;
#13226 = FACE_OUTER_BOUND ( 'NONE', #12521, .T. ) ;
#13227 = VERTEX_POINT ( 'NONE', #13253 ) ;
#13228 = DIRECTION ( 'NONE',  ( 0.000000000000000000, 0.000000000000000000, 1.000000000000000000 ) ) ;
#13229 = VERTEX_POINT ( 'NONE', #10820 ) ;
#13230 = EDGE_CURVE ( 'NONE', #2908, #3918, #998, .T. ) ;
#13231 = DIRECTION ( 'NONE',  ( -1.000000000000000000, 0.000000000000000000, 0.000000000000000000 ) ) ;
#13232 = DIRECTION ( 'NONE',  ( 1.000000000000000000, 0.000000000000000000, 0.000000000000000000 ) ) ;
#13233 = ORIENTED_EDGE ( 'NONE', *, *, #8305, .F. ) ;
#13234 = DIRECTION ( 'NONE',  ( -1.000000000000000000, 0.000000000000000000, 0.000000000000000000 ) ) ;
#13235 = EDGE_CURVE ( 'NONE', #9892, #3062, #12879, .T. ) ;
#13236 = AXIS2_PLACEMENT_3D ( 'NONE', #2723, #6124, #8415 ) ;
#13237 = CARTESIAN_POINT ( 'NONE',  ( -4.999999999999996447, 85.00000000000000000, 46.00000000000000000 ) ) ;
#13238 = ORIENTED_EDGE ( 'NONE', *, *, #4589, .F. ) ;
#13239 = CARTESIAN_POINT ( 'NONE',  ( 2.449293598294700991E-16, -97.00000000000000000, -10.50000000000000000 ) ) ;
#13240 = ORIENTED_EDGE ( 'NONE', *, *, #2918, .F. ) ;
#13241 = DIRECTION ( 'NONE',  ( -1.000000000000000000, 0.000000000000000000, -0.000000000000000000 ) ) ;
#13242 = CARTESIAN_POINT ( 'NONE',  ( 0.000000000000000000, 0.000000000000000000, -8.000000000000000000 ) ) ;
#13243 = CARTESIAN_POINT ( 'NONE',  ( -32.26435573746199736, 42.04772703543562073, 10.49999999999999822 ) ) ;
#13244 = CARTESIAN_POINT ( 'NONE',  ( 48.29629131445336299, 12.94095225512623060, -8.000000000000000000 ) ) ;
#13245 = CARTESIAN_POINT ( 'NONE',  ( -30.80502811811232888, -49.00442420935981147, -10.50000000000000000 ) ) ;
#13246 = VERTEX_POINT ( 'NONE', #2698 ) ;
#13247 = DIRECTION ( 'NONE',  ( -0.000000000000000000, -0.000000000000000000, 1.000000000000000000 ) ) ;
#13248 = CARTESIAN_POINT ( 'NONE',  ( 12.39897948556635754, 100.2360479454198696, 16.00000000000000000 ) ) ;
#13249 = UNCERTAINTY_MEASURE_WITH_UNIT (LENGTH_MEASURE( 1.000000000000000082E-05 ), #908, 'distance_accuracy_value', 'NONE');
#13250 = DIRECTION ( 'NONE',  ( 0.000000000000000000, 0.000000000000000000, -1.000000000000000000 ) ) ;
#13251 = AXIS2_PLACEMENT_3D ( 'NONE', #13172, #14157, #3766 ) ;
#13252 = ORIENTED_EDGE ( 'NONE', *, *, #3041, .T. ) ;
#13253 = CARTESIAN_POINT ( 'NONE',  ( -68.49330278050074128, 68.09867107463051639, 10.49999999999999822 ) ) ;
#13254 = EDGE_CURVE ( 'NONE', #5756, #836, #7043, .T. ) ;
#13255 = ORIENTED_EDGE ( 'NONE', *, *, #7630, .T. ) ;
#13256 = EDGE_CURVE ( 'NONE', #8372, #5320, #13356, .T. ) ;
#13257 = CARTESIAN_POINT ( 'NONE',  ( 29.51438936481373077, 47.21331623427104063, -13.00000000000000178 ) ) ;
#13258 = CARTESIAN_POINT ( 'NONE',  ( -45.91029614918924295, 26.00011991137363765, -10.50000000000000000 ) ) ;
#13259 = EDGE_CURVE ( 'NONE', #4441, #1935, #8737, .T. ) ;
#13260 = DIRECTION ( 'NONE',  ( 1.000000000000000000, 0.000000000000000000, 0.000000000000000000 ) ) ;
#13261 = PLANE ( 'NONE',  #14376 ) ;
#13262 = DIRECTION ( 'NONE',  ( 6.123233995736766036E-17, 0.000000000000000000, 1.000000000000000000 ) ) ;
#13263 = DIRECTION ( 'NONE',  ( 1.000000000000000000, 0.000000000000000000, 0.000000000000000000 ) ) ;
#13264 = CIRCLE ( 'NONE', #12777, 52.50000000000000711 ) ;
#13265 = ORIENTED_EDGE ( 'NONE', *, *, #6151, .T. ) ;
#13266 = EDGE_CURVE ( 'NONE', #2530, #9923, #2203, .T. ) ;
#13267 = DIRECTION ( 'NONE',  ( 1.000000000000000000, 0.000000000000000000, 0.000000000000000000 ) ) ;
#13268 = LINE ( 'NONE', #7328, #606 ) ;
#13269 = DIRECTION ( 'NONE',  ( -1.000000000000000000, 0.000000000000000000, 0.000000000000000000 ) ) ;
#13270 = ORIENTED_EDGE ( 'NONE', *, *, #5595, .T. ) ;
#13271 = ORIENTED_EDGE ( 'NONE', *, *, #10747, .T. ) ;
#13272 = PLANE ( 'NONE',  #9558 ) ;
#13273 = ORIENTED_EDGE ( 'NONE', *, *, #13397, .F. ) ;
#13274 = EDGE_CURVE ( 'NONE', #7460, #7416, #4154, .T. ) ;
#13275 = CARTESIAN_POINT ( 'NONE',  ( 23.51438936481372366, 47.21331623427104063, -8.000000000000000000 ) ) ;
#13276 = CARTESIAN_POINT ( 'NONE',  ( -3.999999999999996447, -2.309401076758511806, -3.433295621305381573 ) ) ;
#13277 = DIRECTION ( 'NONE',  ( 1.000000000000000000, 0.000000000000000000, 0.000000000000000000 ) ) ;
#13278 = CARTESIAN_POINT ( 'NONE',  ( -50.00000000000000000, 0.000000000000000000, 13.00000000000000178 ) ) ;
#13279 = VERTEX_POINT ( 'NONE', #5125 ) ;
#13280 = FACE_OUTER_BOUND ( 'NONE', #13895, .T. ) ;
#13281 = ORIENTED_EDGE ( 'NONE', *, *, #3887, .T. ) ;
#13282 = EDGE_LOOP ( 'NONE', ( #7950, #5366, #14287, #12984 ) ) ;
#13283 = DIRECTION ( 'NONE',  ( 0.000000000000000000, 0.000000000000000000, -1.000000000000000000 ) ) ;
#13284 = CARTESIAN_POINT ( 'NONE',  ( 36.08010649850015739, 100.2464683348682541, -16.00000000000000000 ) ) ;
#13285 = CARTESIAN_POINT ( 'NONE',  ( -43.30127018922183169, 25.00000000000018474, 8.000000000000000000 ) ) ;
#13286 = DIRECTION ( 'NONE',  ( 0.000000000000000000, 0.000000000000000000, -1.000000000000000000 ) ) ;
#13287 = CARTESIAN_POINT ( 'NONE',  ( 4.211140560182194292, 2.431303136016534250, -3.745885042887433958 ) ) ;
#13288 = DIRECTION ( 'NONE',  ( 1.000000000000000000, 0.000000000000000000, 0.000000000000000000 ) ) ;
#13289 = VERTEX_POINT ( 'NONE', #9657 ) ;
#13290 = ADVANCED_FACE ( 'NONE', ( #14386 ), #8534, .F. ) ;
#13291 = CARTESIAN_POINT ( 'NONE',  ( 0.000000000000000000, 0.000000000000000000, 4.000000000000000000 ) ) ;
#13292 = DIRECTION ( 'NONE',  ( 0.000000000000000000, 0.000000000000000000, 1.000000000000000000 ) ) ;
#13293 = DIRECTION ( 'NONE',  ( 0.000000000000000000, 0.000000000000000000, -1.000000000000000000 ) ) ;
#13294 = CARTESIAN_POINT ( 'NONE',  ( -22.33583958711380646, -30.74264578624812927, -28.00000000000000000 ) ) ;
#13295 = VERTEX_POINT ( 'NONE', #13180 ) ;
#13296 = FILL_AREA_STYLE ('',( #2975 ) ) ;
#13297 = ORIENTED_EDGE ( 'NONE', *, *, #9314, .F. ) ;
#13298 = DIRECTION ( 'NONE',  ( -1.000000000000000000, 0.000000000000000000, -0.000000000000000000 ) ) ;
#13299 = ORIENTED_EDGE ( 'NONE', *, *, #12806, .F. ) ;
#13300 = DIRECTION ( 'NONE',  ( -1.000000000000000000, 0.000000000000000000, 0.000000000000000000 ) ) ;
#13301 = ORIENTED_EDGE ( 'NONE', *, *, #4262, .F. ) ;
#13302 = CARTESIAN_POINT ( 'NONE',  ( 12.86891638962116247, -56.43380494354001087, -10.50000000000000000 ) ) ;
#13303 = DIRECTION ( 'NONE',  ( -0.000000000000000000, -0.000000000000000000, -1.000000000000000000 ) ) ;
#13304 = DIRECTION ( 'NONE',  ( 1.000000000000000000, 0.000000000000000000, 0.000000000000000000 ) ) ;
#13305 = DIRECTION ( 'NONE',  ( 0.000000000000000000, 0.000000000000000000, 1.000000000000000000 ) ) ;
#13306 = EDGE_CURVE ( 'NONE', #1631, #8562, #8019, .T. ) ;
#13307 = CARTESIAN_POINT ( 'NONE',  ( 0.000000000000000000, 0.000000000000000000, 8.000000000000000000 ) ) ;
#13308 = ADVANCED_FACE ( 'NONE', ( #13317 ), #6533, .F. ) ;
#13309 = EDGE_CURVE ( 'NONE', #6495, #9289, #13136, .T. ) ;
#13310 = DIRECTION ( 'NONE',  ( 1.000000000000000000, 0.000000000000000000, 0.000000000000000000 ) ) ;
#13311 = ORIENTED_EDGE ( 'NONE', *, *, #6107, .F. ) ;
#13312 = DIRECTION ( 'NONE',  ( 0.000000000000000000, 0.000000000000000000, 1.000000000000000000 ) ) ;
#13313 = CARTESIAN_POINT ( 'NONE',  ( 14.07862063237891981, -50.84834283436993729, -13.00000000000000178 ) ) ;
#13314 = CARTESIAN_POINT ( 'NONE',  ( 4.197478902586991190, -0.8524102783748379597, -3.505063281295504929 ) ) ;
#13315 = ORIENTED_EDGE ( 'NONE', *, *, #7634, .F. ) ;
#13316 = EDGE_LOOP ( 'NONE', ( #14109, #9673 ) ) ;
#13317 = FACE_OUTER_BOUND ( 'NONE', #10371, .T. ) ;
#13318 = ORIENTED_EDGE ( 'NONE', *, *, #11427, .T. ) ;
#13319 = CARTESIAN_POINT ( 'NONE',  ( -94.51066581171356518, -1.674280531758327140, 8.000000000000000000 ) ) ;
#13320 = DIRECTION ( 'NONE',  ( 1.000000000000000000, 0.000000000000000000, 0.000000000000000000 ) ) ;
#13321 = CARTESIAN_POINT ( 'NONE',  ( -69.16568774265545017, 71.53347797788843820, -8.000000000000000000 ) ) ;
#13322 = DIRECTION ( 'NONE',  ( 0.000000000000000000, 0.000000000000000000, 1.000000000000000000 ) ) ;
#13323 = DIRECTION ( 'NONE',  ( 1.000000000000000000, 0.000000000000000000, 0.000000000000000000 ) ) ;
#13324 = ORIENTED_EDGE ( 'NONE', *, *, #5016, .F. ) ;
#13325 = ORIENTED_EDGE ( 'NONE', *, *, #7198, .F. ) ;
#13326 = CIRCLE ( 'NONE', #8708, 3.000000000000002665 ) ;
#13327 = ORIENTED_EDGE ( 'NONE', *, *, #13735, .F. ) ;
#13328 = CARTESIAN_POINT ( 'NONE',  ( 2.449293598294700991E-16, -97.00000000000000000, 10.49999999999999822 ) ) ;
#13329 = VECTOR ( 'NONE', #2575, 1000.000000000000000 ) ;
#13330 = CARTESIAN_POINT ( 'NONE',  ( 57.06275842387049835, -9.706953719245678514, -13.00000000000000178 ) ) ;
#13331 = EDGE_CURVE ( 'NONE', #14691, #5358, #7695, .T. ) ;
#13332 = VECTOR ( 'NONE', #3115, 1000.000000000000000 ) ;
#13333 = FACE_OUTER_BOUND ( 'NONE', #7930, .T. ) ;
#13334 = ORIENTED_EDGE ( 'NONE', *, *, #8795, .F. ) ;
#13335 = ADVANCED_FACE ( 'NONE', ( #5349 ), #6472, .F. ) ;
#13336 = ORIENTED_EDGE ( 'NONE', *, *, #14648, .T. ) ;
#13337 = VERTEX_POINT ( 'NONE', #5011 ) ;
#13338 = ORIENTED_EDGE ( 'NONE', *, *, #382, .F. ) ;
#13339 = CIRCLE ( 'NONE', #8718, 2.649999999999992806 ) ;
#13340 = CIRCLE ( 'NONE', #2188, 60.50000000000000000 ) ;
#13341 = DIRECTION ( 'NONE',  ( 1.000000000000000000, 0.000000000000000000, 0.000000000000000000 ) ) ;
#13342 = VECTOR ( 'NONE', #1469, 1000.000000000000000 ) ;
#13343 = COLOUR_RGB ( '', 0.40784314, 0.44705882, 0.49803922) ;
#13344 = DIRECTION ( 'NONE',  ( 1.000000000000000000, 0.000000000000000000, 0.000000000000000000 ) ) ;
#13345 = VERTEX_POINT ( 'NONE', #11277 ) ;
#13346 = CARTESIAN_POINT ( 'NONE',  ( 9.714003807514266953, 53.63365512954683112, -13.00000000000000178 ) ) ;
#13347 = CARTESIAN_POINT ( 'NONE',  ( 51.19406879332056093, 13.71740939043382745, 8.000000000000000000 ) ) ;
#13348 = ORIENTED_EDGE ( 'NONE', *, *, #9226, .T. ) ;
#13349 = CARTESIAN_POINT ( 'NONE',  ( -42.04772703543551415, -32.26435573746212526, 8.000000000000000000 ) ) ;
#13350 = EDGE_CURVE ( 'NONE', #13058, #6851, #2459, .T. ) ;
#13351 = AXIS2_PLACEMENT_3D ( 'NONE', #4791, #13065, #2813 ) ;
#13352 = EDGE_CURVE ( 'NONE', #11311, #12963, #1972, .T. ) ;
#13353 = ORIENTED_EDGE ( 'NONE', *, *, #539, .T. ) ;
#13354 = VECTOR ( 'NONE', #3512, 1000.000000000000000 ) ;
#13355 = CIRCLE ( 'NONE', #263, 100.0000000000000000 ) ;
#13356 = CIRCLE ( 'NONE', #6791, 0.2500000000000002220 ) ;
#13357 = ORIENTED_EDGE ( 'NONE', *, *, #6088, .T. ) ;
#13358 = CARTESIAN_POINT ( 'NONE',  ( 45.89934640057532533, -26.49999999999987566, -10.50000000000000000 ) ) ;
#13359 = FACE_OUTER_BOUND ( 'NONE', #13834, .T. ) ;
#13360 = EDGE_CURVE ( 'NONE', #12781, #4070, #12410, .T. ) ;
#13361 = CARTESIAN_POINT ( 'NONE',  ( 0.000000000000000000, 0.000000000000000000, -8.000000000000000000 ) ) ;
#13362 = CARTESIAN_POINT ( 'NONE',  ( 89.61631465359491244, 37.12029293941346708, -13.00000000000000178 ) ) ;
#13363 = DIRECTION ( 'NONE',  ( 1.000000000000000000, -4.440892098500626162E-15, 0.000000000000000000 ) ) ;
#13364 = AXIS2_PLACEMENT_3D ( 'NONE', #14023, #11749, #11677 ) ;
#13365 = DIRECTION ( 'NONE',  ( 0.000000000000000000, 0.000000000000000000, 1.000000000000000000 ) ) ;
#13366 = AXIS2_PLACEMENT_3D ( 'NONE', #6850, #11513, #5784 ) ;
#13367 = ORIENTED_EDGE ( 'NONE', *, *, #11829, .F. ) ;
#13368 = DIRECTION ( 'NONE',  ( -0.000000000000000000, -0.000000000000000000, -1.000000000000000000 ) ) ;
#13369 = PRODUCT_DEFINITION_SHAPE ( 'NONE', 'NONE',  #8937 ) ;
#13370 = FACE_OUTER_BOUND ( 'NONE', #10591, .T. ) ;
#13371 = CARTESIAN_POINT ( 'NONE',  ( -2.449293598294708880E-16, 38.00000000000000000, -25.50000000000000355 ) ) ;
#13372 = CARTESIAN_POINT ( 'NONE',  ( 32.06294366074496338, -42.50536573064421475, 10.49999999999999822 ) ) ;
#13373 = CIRCLE ( 'NONE', #12401, 53.55662432702593634 ) ;
#13374 = VERTEX_POINT ( 'NONE', #11349 ) ;
#13375 = CARTESIAN_POINT ( 'NONE',  ( 29.95202887341198661, 96.45668229681564299, -12.61733007774791560 ) ) ;
#13376 = DIRECTION ( 'NONE',  ( 0.000000000000000000, 0.000000000000000000, -1.000000000000000000 ) ) ;
#13377 = ORIENTED_EDGE ( 'NONE', *, *, #14050, .T. ) ;
#13378 = CARTESIAN_POINT ( 'NONE',  ( -89.61631465359519666, -37.12029293941281338, 8.000000000000000000 ) ) ;
#13379 = ORIENTED_EDGE ( 'NONE', *, *, #13397, .T. ) ;
#13380 = CARTESIAN_POINT ( 'NONE',  ( 11.26445476358325237, 106.4056658731563942, 18.30680964731275040 ) ) ;
#13381 = DIRECTION ( 'NONE',  ( 0.000000000000000000, 0.000000000000000000, 1.000000000000000000 ) ) ;
#13382 = CYLINDRICAL_SURFACE ( 'NONE', #7329, 59.50000000000000000 ) ;
#13383 = AXIS2_PLACEMENT_3D ( 'NONE', #3358, #943, #4435 ) ;
#13384 = CYLINDRICAL_SURFACE ( 'NONE', #5346, 2.649999999999992806 ) ;
#13385 = CARTESIAN_POINT ( 'NONE',  ( 68.68541276968825571, -69.08004447556089644, -10.50000000000000000 ) ) ;
#13386 = ORIENTED_EDGE ( 'NONE', *, *, #13066, .T. ) ;
#13387 = CARTESIAN_POINT ( 'NONE',  ( -11.63111172283970518, 94.28541358805125583, 17.83102282485376833 ) ) ;
#13388 = ORIENTED_EDGE ( 'NONE', *, *, #10332, .F. ) ;
#13389 = AXIS2_PLACEMENT_3D ( 'NONE', #7845, #2088, #3153 ) ;
#13390 = CARTESIAN_POINT ( 'NONE',  ( 11.47770164139309124, 74.11716252799973859, -18.08381726540839196 ) ) ;
#13391 = CARTESIAN_POINT ( 'NONE',  ( -32.26435573746199736, 42.04772703543562073, -13.00000000000000178 ) ) ;
#13392 = CARTESIAN_POINT ( 'NONE',  ( 3.999999999999998224, -0.8578082829537109211, -3.433262215449996102 ) ) ;
#13393 = EDGE_CURVE ( 'NONE', #13059, #5144, #9244, .T. ) ;
#13394 = CIRCLE ( 'NONE', #6838, 3.000000000000002665 ) ;
#13395 = ORIENTED_EDGE ( 'NONE', *, *, #1154, .F. ) ;
#13396 = EDGE_CURVE ( 'NONE', #5665, #1495, #11430, .T. ) ;
#13397 = EDGE_CURVE ( 'NONE', #2518, #7149, #6568, .T. ) ;
#13398 = CARTESIAN_POINT ( 'NONE',  ( -2.756197834950063097, -3.027510591568736142, -3.223146290109811130 ) ) ;
#13399 = ORIENTED_EDGE ( 'NONE', *, *, #12875, .T. ) ;
#13400 = VECTOR ( 'NONE', #12717, 1000.000000000000000 ) ;
#13401 = CARTESIAN_POINT ( 'NONE',  ( 26.49999999999971578, 45.89934640057541060, -13.00000000000000178 ) ) ;
#13402 = CARTESIAN_POINT ( 'NONE',  ( -45.89934640057513349, 26.50000000000019540, -8.000000000000000000 ) ) ;
#13403 = DIRECTION ( 'NONE',  ( -1.000000000000000000, 0.000000000000000000, 0.000000000000000000 ) ) ;
#13404 = DIRECTION ( 'NONE',  ( 0.000000000000000000, 0.000000000000000000, -1.000000000000000000 ) ) ;
#13405 = DIRECTION ( 'NONE',  ( 0.000000000000000000, 0.000000000000000000, 1.000000000000000000 ) ) ;
#13406 = VERTEX_POINT ( 'NONE', #7920 ) ;
#13407 = ORIENTED_EDGE ( 'NONE', *, *, #7773, .T. ) ;
#13408 = VERTEX_POINT ( 'NONE', #2150 ) ;
#13409 = CIRCLE ( 'NONE', #1297, 63.00000000000000000 ) ;
#13410 = DIRECTION ( 'NONE',  ( -0.000000000000000000, -0.000000000000000000, 1.000000000000000000 ) ) ;
#13411 = DIRECTION ( 'NONE',  ( 0.000000000000000000, 0.000000000000000000, 1.000000000000000000 ) ) ;
#13412 = EDGE_CURVE ( 'NONE', #3540, #15011, #803, .T. ) ;
#13413 = CARTESIAN_POINT ( 'NONE',  ( 30.80502811811196295, 49.00442420936003174, 8.000000000000000000 ) ) ;
#13414 = VERTEX_POINT ( 'NONE', #13474 ) ;
#13415 = AXIS2_PLACEMENT_3D ( 'NONE', #3698, #12957, #11822 ) ;
#13416 = ORIENTED_EDGE ( 'NONE', *, *, #6715, .T. ) ;
#13417 = EDGE_CURVE ( 'NONE', #11178, #4704, #14106, .T. ) ;
#13418 = VERTEX_POINT ( 'NONE', #14845 ) ;
#13419 = CIRCLE ( 'NONE', #328, 59.50000000000000000 ) ;
#13420 = FACE_OUTER_BOUND ( 'NONE', #2251, .T. ) ;
#13421 = DIRECTION ( 'NONE',  ( -1.000000000000000000, 0.000000000000000000, 0.000000000000000000 ) ) ;
#13422 = CARTESIAN_POINT ( 'NONE',  ( -31.05588327715806329, 44.79355920668842828, -13.00000000000000178 ) ) ;
#13423 = EDGE_LOOP ( 'NONE', ( #6959, #8701, #10134, #13315 ) ) ;
#13424 = AXIS2_PLACEMENT_3D ( 'NONE', #4374, #5436, #11128 ) ;
#13425 = DIRECTION ( 'NONE',  ( 1.000000000000000000, 0.000000000000000000, 0.000000000000000000 ) ) ;
#13426 = CARTESIAN_POINT ( 'NONE',  ( -31.47058823529412663, 102.2673069760056421, 11.00000000000000000 ) ) ;
#13427 = ORIENTED_EDGE ( 'NONE', *, *, #6417, .F. ) ;
#13428 = CARTESIAN_POINT ( 'NONE',  ( 0.000000000000000000, 0.000000000000000000, 8.000000000000000000 ) ) ;
#13429 = VERTEX_POINT ( 'NONE', #4445 ) ;
#13430 = VERTEX_POINT ( 'NONE', #3080 ) ;
#13431 = CIRCLE ( 'NONE', #14904, 0.5000000000000004441 ) ;
#13432 = CARTESIAN_POINT ( 'NONE',  ( -30.19044911324211000, 96.38232397946877938, 13.21859331841449858 ) ) ;
#13433 = CIRCLE ( 'NONE', #6874, 75.00000000000001421 ) ;
#13434 = AXIS2_PLACEMENT_3D ( 'NONE', #6532, #12177, #7687 ) ;
#13435 = DIRECTION ( 'NONE',  ( 1.000000000000000000, 0.000000000000000000, 0.000000000000000000 ) ) ;
#13436 = ADVANCED_FACE ( 'NONE', ( #9054 ), #12339, .F. ) ;
#13437 = ADVANCED_FACE ( 'NONE', ( #6764 ), #4522, .T. ) ;
#13438 = CARTESIAN_POINT ( 'NONE',  ( 5.560781378645573980, 6.809993116116507654E-16, -4.000000000000000000 ) ) ;
#13439 = CARTESIAN_POINT ( 'NONE',  ( 45.89934640057532533, -26.49999999999987566, -8.000000000000000000 ) ) ;
#13440 = CARTESIAN_POINT ( 'NONE',  ( 0.000000000000000000, 0.000000000000000000, 8.000000000000000000 ) ) ;
#13441 = EDGE_CURVE ( 'NONE', #13246, #14727, #3924, .T. ) ;
#13442 = ORIENTED_EDGE ( 'NONE', *, *, #11687, .F. ) ;
#13443 = AXIS2_PLACEMENT_3D ( 'NONE', #159, #11784, #9626 ) ;
#13444 = AXIS2_PLACEMENT_3D ( 'NONE', #3687, #9434, #5733 ) ;
#13445 = DIRECTION ( 'NONE',  ( 0.000000000000000000, 0.000000000000000000, -1.000000000000000000 ) ) ;
#13446 = AXIS2_PLACEMENT_3D ( 'NONE', #6416, #11071, #13341 ) ;
#13447 = EDGE_CURVE ( 'NONE', #3890, #8922, #4167, .T. ) ;
#13448 = CARTESIAN_POINT ( 'NONE',  ( 0.000000000000000000, 0.000000000000000000, 14.49999999999999822 ) ) ;
#13449 = CARTESIAN_POINT ( 'NONE',  ( 4.197393957002300446, 7.760817478283647932E-14, -3.503767560748928922 ) ) ;
#13450 = ORIENTED_EDGE ( 'NONE', *, *, #10791, .F. ) ;
#13451 = DIRECTION ( 'NONE',  ( 1.000000000000000000, 0.000000000000000000, 0.000000000000000000 ) ) ;
#13452 = ORIENTED_EDGE ( 'NONE', *, *, #686, .F. ) ;
#13453 = DIRECTION ( 'NONE',  ( -1.000000000000000000, 0.000000000000000000, 0.000000000000000000 ) ) ;
#13454 = ORIENTED_EDGE ( 'NONE', *, *, #1248, .T. ) ;
#13455 = AXIS2_PLACEMENT_3D ( 'NONE', #8536, #14164, #8609 ) ;
#13456 = CYLINDRICAL_SURFACE ( 'NONE', #6538, 0.5000000000000004441 ) ;
#13457 = EDGE_LOOP ( 'NONE', ( #12744, #10171, #14239, #10849, #12142, #14882 ) ) ;
#13458 = EDGE_CURVE ( 'NONE', #2743, #8664, #12406, .T. ) ;
#13459 = ORIENTED_EDGE ( 'NONE', *, *, #11143, .F. ) ;
#13460 = DIRECTION ( 'NONE',  ( 1.000000000000000000, 0.000000000000000000, 0.000000000000000000 ) ) ;
#13461 = DIRECTION ( 'NONE',  ( 1.000000000000000000, 0.000000000000000000, 0.000000000000000000 ) ) ;
#13462 = DIRECTION ( 'NONE',  ( 0.000000000000000000, 0.000000000000000000, 1.000000000000000000 ) ) ;
#13463 = LINE ( 'NONE', #6608, #4592 ) ;
#13464 = DIRECTION ( 'NONE',  ( 0.000000000000000000, 0.000000000000000000, 1.000000000000000000 ) ) ;
#13465 = CARTESIAN_POINT ( 'NONE',  ( -39.04772703543551415, -32.26435573746212526, 8.000000000000000000 ) ) ;
#13466 = AXIS2_PLACEMENT_3D ( 'NONE', #10258, #6906, #5548 ) ;
#13467 = ORIENTED_EDGE ( 'NONE', *, *, #3411, .F. ) ;
#13468 = FACE_OUTER_BOUND ( 'NONE', #7323, .T. ) ;
#13469 = CARTESIAN_POINT ( 'NONE',  ( 0.000000000000000000, 0.000000000000000000, -23.50000000000000000 ) ) ;
#13470 = AXIS2_PLACEMENT_3D ( 'NONE', #11242, #4488, #6667 ) ;
#13471 = CARTESIAN_POINT ( 'NONE',  ( 4.204115023516828309, -1.660442669500202140, -3.602151381774573391 ) ) ;
#13472 = ORIENTED_EDGE ( 'NONE', *, *, #14506, .T. ) ;
#13473 = AXIS2_PLACEMENT_3D ( 'NONE', #8540, #2783, #6250 ) ;
#13474 = CARTESIAN_POINT ( 'NONE',  ( 14.00000000000000000, 1.714505518806294638E-15, -45.50000000000000000 ) ) ;
#13475 = ORIENTED_EDGE ( 'NONE', *, *, #921, .T. ) ;
#13476 = CYLINDRICAL_SURFACE ( 'NONE', #5222, 0.5000000000000004441 ) ;
#13477 = FILL_AREA_STYLE_COLOUR ( '', #7307 ) ;
#13478 = DIRECTION ( 'NONE',  ( 0.000000000000000000, 0.000000000000000000, 1.000000000000000000 ) ) ;
#13479 = DIRECTION ( 'NONE',  ( 0.000000000000000000, 0.000000000000000000, -1.000000000000000000 ) ) ;
#13480 = CARTESIAN_POINT ( 'NONE',  ( 0.000000000000000000, 0.000000000000000000, 37.00000000000000711 ) ) ;
#13481 = ORIENTED_EDGE ( 'NONE', *, *, #12291, .F. ) ;
#13482 = ORIENTED_EDGE ( 'NONE', *, *, #1008, .F. ) ;
#13483 = ADVANCED_FACE ( 'NONE', ( #100 ), #5720, .T. ) ;
#13484 = AXIS2_PLACEMENT_3D ( 'NONE', #12946, #8226, #8529 ) ;
#13485 = CARTESIAN_POINT ( 'NONE',  ( 30.80502811811196295, 49.00442420936003174, -13.00000000000000178 ) ) ;
#13487 = EDGE_CURVE ( 'NONE', #5269, #2264, #9358, .T. ) ;
#13486 = CARTESIAN_POINT ( 'NONE',  ( 8.075974454121990220, 94.65787058575050139, 19.99999999999999289 ) ) ;
#13488 = CARTESIAN_POINT ( 'NONE',  ( -30.80502811811232888, -49.00442420935981147, 8.000000000000000000 ) ) ;
#13489 = ORIENTED_EDGE ( 'NONE', *, *, #14971, .T. ) ;
#13490 = VERTEX_POINT ( 'NONE', #6007 ) ;
#13491 = ORIENTED_EDGE ( 'NONE', *, *, #7882, .T. ) ;
#13492 = AXIS2_PLACEMENT_3D ( 'NONE', #6950, #4614, #1054 ) ;
#13493 = AXIS2_PLACEMENT_3D ( 'NONE', #9047, #2368, #10414 ) ;
#13494 = DIRECTION ( 'NONE',  ( 1.000000000000000000, 0.000000000000000000, 0.000000000000000000 ) ) ;
#13495 = PRODUCT_DEFINITION_SHAPE ( 'NONE', 'NONE',  #9593 ) ;
#13496 = PLANE ( 'NONE',  #7362 ) ;
#13497 = EDGE_CURVE ( 'NONE', #6488, #9994, #2704, .T. ) ;
#13498 = CARTESIAN_POINT ( 'NONE',  ( -68.08935777509570642, -68.58935777509452691, -10.50000000000000000 ) ) ;
#13499 = FACE_OUTER_BOUND ( 'NONE', #1956, .T. ) ;
#13500 = CARTESIAN_POINT ( 'NONE',  ( -31.47058823529411953, 102.2673069760056421, 11.33189534135684973 ) ) ;
#13501 = ORIENTED_EDGE ( 'NONE', *, *, #9226, .F. ) ;
#13502 = ADVANCED_FACE ( 'NONE', ( #11804 ), #6925, .F. ) ;
#13503 = ADVANCED_FACE ( 'NONE', ( #2448 ), #7067, .T. ) ;
#13504 = DIRECTION ( 'NONE',  ( 0.000000000000000000, 0.000000000000000000, -1.000000000000000000 ) ) ;
#13505 = ORIENTED_EDGE ( 'NONE', *, *, #2771, .F. ) ;
#13506 = ORIENTED_EDGE ( 'NONE', *, *, #11366, .T. ) ;
#13507 = CARTESIAN_POINT ( 'NONE',  ( 20.00000000000000000, 2.449293598294706513E-15, -25.50000000000000355 ) ) ;
#13508 = DIRECTION ( 'NONE',  ( -0.000000000000000000, -0.000000000000000000, -1.000000000000000000 ) ) ;
#13509 = CARTESIAN_POINT ( 'NONE',  ( -49.11971303961688307, -15.88467684210530528, 8.000000000000000000 ) ) ;
#13510 = DIRECTION ( 'NONE',  ( 0.000000000000000000, 0.000000000000000000, -1.000000000000000000 ) ) ;
#13511 = DIRECTION ( 'NONE',  ( 1.000000000000000000, 0.000000000000000000, 0.000000000000000000 ) ) ;
#13512 = EDGE_LOOP ( 'NONE', ( #8267, #5738, #7095, #7628, #9001, #14863, #2498, #4746 ) ) ;
#13513 = DIRECTION ( 'NONE',  ( 1.000000000000000000, 0.000000000000000000, 0.000000000000000000 ) ) ;
#13514 = VERTEX_POINT ( 'NONE', #5940 ) ;
#13515 = DIRECTION ( 'NONE',  ( -1.000000000000000000, 0.000000000000000000, 0.000000000000000000 ) ) ;
#13516 = CARTESIAN_POINT ( 'NONE',  ( 0.000000000000000000, 0.000000000000000000, 8.000000000000000000 ) ) ;
#13517 = EDGE_CURVE ( 'NONE', #8108, #11288, #1322, .T. ) ;
#13518 = ORIENTED_EDGE ( 'NONE', *, *, #2780, .F. ) ;
#13519 = DIRECTION ( 'NONE',  ( 0.000000000000000000, 0.000000000000000000, -1.000000000000000000 ) ) ;
#13520 = ORIENTED_EDGE ( 'NONE', *, *, #5699, .F. ) ;
#13521 = DIRECTION ( 'NONE',  ( 1.000000000000000000, 0.000000000000000000, 0.000000000000000000 ) ) ;
#13522 = ADVANCED_FACE ( 'NONE', ( #10578 ), #10354, .F. ) ;
#13523 = VERTEX_POINT ( 'NONE', #176 ) ;
#13524 = FACE_OUTER_BOUND ( 'NONE', #11431, .T. ) ;
#13525 = ORIENTED_EDGE ( 'NONE', *, *, #5082, .T. ) ;
#13526 = CARTESIAN_POINT ( 'NONE',  ( -2.449293598294700991E-16, 97.00000000000000000, 10.49999999999999822 ) ) ;
#13527 = CARTESIAN_POINT ( 'NONE',  ( 90.10640870805727332, 37.02125851216391794, 10.49999999999999822 ) ) ;
#13528 = CARTESIAN_POINT ( 'NONE',  ( -9.706953719245875689, -57.06275842387046993, 8.000000000000000000 ) ) ;
#13529 = ADVANCED_FACE ( 'NONE', ( #14070 ), #10641, .F. ) ;
#13530 = FACE_OUTER_BOUND ( 'NONE', #6849, .T. ) ;
#13531 = LINE ( 'NONE', #14688, #4958 ) ;
#13532 = ORIENTED_EDGE ( 'NONE', *, *, #4139, .T. ) ;
#13533 = PRESENTATION_STYLE_ASSIGNMENT (( #7757 ) ) ;
#13534 = ORIENTED_EDGE ( 'NONE', *, *, #10723, .T. ) ;
#13535 = CARTESIAN_POINT ( 'NONE',  ( 90.11631465359491244, 37.12029293941346708, -13.00000000000000178 ) ) ;
#13536 = CARTESIAN_POINT ( 'NONE',  ( 12.26039456458906152, 94.20559340471635323, -16.55589812076405209 ) ) ;
#13537 = EDGE_CURVE ( 'NONE', #1631, #2976, #5131, .T. ) ;
#13538 = EDGE_CURVE ( 'NONE', #12429, #12179, #1741, .T. ) ;
#13539 = DIRECTION ( 'NONE',  ( 0.000000000000000000, 0.000000000000000000, 1.000000000000000000 ) ) ;
#13540 = DIRECTION ( 'NONE',  ( -1.000000000000000000, 0.000000000000000000, 0.000000000000000000 ) ) ;
#13541 = ORIENTED_EDGE ( 'NONE', *, *, #8566, .F. ) ;
#13542 = CARTESIAN_POINT ( 'NONE',  ( 12.39897948556635754, 61.76783392443436327, 16.00000000000000000 ) ) ;
#13543 = ORIENTED_EDGE ( 'NONE', *, *, #8446, .T. ) ;
#13544 = CYLINDRICAL_SURFACE ( 'NONE', #3527, 0.5000000000000038858 ) ;
#13545 = CARTESIAN_POINT ( 'NONE',  ( -51.19406879332065330, -13.71740939043347041, -8.000000000000000000 ) ) ;
#13546 = EDGE_CURVE ( 'NONE', #3127, #14249, #3436, .T. ) ;
#13547 = CARTESIAN_POINT ( 'NONE',  ( 10.80089892394231832, 106.4537193389066374, -18.76964747820620261 ) ) ;
#13548 = CARTESIAN_POINT ( 'NONE',  ( 0.000000000000000000, 0.000000000000000000, -10.50000000000000000 ) ) ;
#13549 = APPLICATION_PROTOCOL_DEFINITION ( 'draft international standard', 'automotive_design', 1998, #6968 ) ;
#13550 = ORIENTED_EDGE ( 'NONE', *, *, #8898, .F. ) ;
#13551 = VERTEX_POINT ( 'NONE', #10500 ) ;
#13552 = VERTEX_POINT ( 'NONE', #12713 ) ;
#13553 = DIRECTION ( 'NONE',  ( -0.000000000000000000, -0.000000000000000000, 1.000000000000000000 ) ) ;
#13554 = DIRECTION ( 'NONE',  ( 1.000000000000000000, 0.000000000000000000, 0.000000000000000000 ) ) ;
#13555 = DIRECTION ( 'NONE',  ( 0.000000000000000000, 0.000000000000000000, -1.000000000000000000 ) ) ;
#13556 = ORIENTED_EDGE ( 'NONE', *, *, #7306, .F. ) ;
#13557 = AXIS2_PLACEMENT_3D ( 'NONE', #314, #13001, #2593 ) ;
#13558 = EDGE_LOOP ( 'NONE', ( #14741, #4419, #10204, #4808 ) ) ;
#13559 = ORIENTED_EDGE ( 'NONE', *, *, #5389, .T. ) ;
#13560 = CARTESIAN_POINT ( 'NONE',  ( -12.50000000000000000, 100.2235002382176248, 15.33678752976415716 ) ) ;
#13561 = FACE_OUTER_BOUND ( 'NONE', #12709, .T. ) ;
#13562 = CARTESIAN_POINT ( 'NONE',  ( 0.000000000000000000, 0.000000000000000000, 0.000000000000000000 ) ) ;
#13563 = DIRECTION ( 'NONE',  ( -0.000000000000000000, -0.000000000000000000, 1.000000000000000000 ) ) ;
#13564 = AXIS2_PLACEMENT_3D ( 'NONE', #6816, #12601, #13904 ) ;
#13565 = CARTESIAN_POINT ( 'NONE',  ( 15.88467684210547226, -49.11971303961683333, -8.000000000000000000 ) ) ;
#13566 = CARTESIAN_POINT ( 'NONE',  ( -31.95756590787640050, 102.1116157579503323, 13.22695225398607732 ) ) ;
#13567 = EDGE_LOOP ( 'NONE', ( #4243, #9099, #4278, #7447, #1354, #5823 ) ) ;
#13568 = VERTEX_POINT ( 'NONE', #9205 ) ;
#13569 = CIRCLE ( 'NONE', #10417, 52.50000000000000711 ) ;
#13570 = VERTEX_POINT ( 'NONE', #4745 ) ;
#13571 = DIRECTION ( 'NONE',  ( 0.000000000000000000, 0.000000000000000000, 1.000000000000000000 ) ) ;
#13572 = VECTOR ( 'NONE', #557, 1000.000000000000000 ) ;
#13573 = ADVANCED_FACE ( 'NONE', ( #13857 ), #11442, .F. ) ;
#13574 = CONICAL_SURFACE ( 'NONE', #2915, 4.000000000000000000, 0.8911886515913786111 ) ;
#13575 = EDGE_CURVE ( 'NONE', #12855, #6102, #12646, .T. ) ;
#13576 = CIRCLE ( 'NONE', #14553, 0.5000000000000073275 ) ;
#13577 = EDGE_CURVE ( 'NONE', #5002, #12160, #1023, .T. ) ;
#13578 = EDGE_CURVE ( 'NONE', #14819, #14961, #9003, .T. ) ;
#13579 = DIRECTION ( 'NONE',  ( -1.000000000000000000, 0.000000000000000000, 0.000000000000000000 ) ) ;
#13580 = DIRECTION ( 'NONE',  ( -0.000000000000000000, -0.000000000000000000, 1.000000000000000000 ) ) ;
#13581 = FACE_OUTER_BOUND ( 'NONE', #4841, .T. ) ;
#13582 = CARTESIAN_POINT ( 'NONE',  ( -68.49330278050074128, 68.09867107463051639, -13.00000000000000178 ) ) ;
#13583 = CIRCLE ( 'NONE', #6774, 3.000000000000002665 ) ;
#13584 = DIRECTION ( 'NONE',  ( 1.000000000000000000, 0.000000000000000000, 0.000000000000000000 ) ) ;
#13585 = ORIENTED_EDGE ( 'NONE', *, *, #12846, .F. ) ;
#13586 = CIRCLE ( 'NONE', #10435, 100.0000000000000000 ) ;
#13587 = CYLINDRICAL_SURFACE ( 'NONE', #6063, 3.000000000000002665 ) ;
#13588 = ORIENTED_EDGE ( 'NONE', *, *, #7358, .F. ) ;
#13589 = STYLED_ITEM ( 'NONE', ( #8261 ), #7823 ) ;
#13590 = DIRECTION ( 'NONE',  ( -1.000000000000000000, 0.000000000000000000, 0.000000000000000000 ) ) ;
#13591 = CARTESIAN_POINT ( 'NONE',  ( -26.01305530232562546, -46.81487971942612347, -10.50000000000000000 ) ) ;
#13592 = EDGE_LOOP ( 'NONE', ( #7843, #12459 ) ) ;
#13593 = CARTESIAN_POINT ( 'NONE',  ( -4.197393957002300446, -7.680494662014190109E-14, -3.503767560748928922 ) ) ;
#13594 = AXIS2_PLACEMENT_3D ( 'NONE', #7668, #7588, #12237 ) ;
#13595 = EDGE_LOOP ( 'NONE', ( #728, #7743, #11184, #12673, #11762, #3773, #2580, #8636, #6206, #2298 ) ) ;
#13596 = AXIS2_PLACEMENT_3D ( 'NONE', #8413, #9538, #2640 ) ;
#13597 = CARTESIAN_POINT ( 'NONE',  ( 89.61631465359491244, 37.12029293941346708, -8.000000000000000000 ) ) ;
#13598 = ORIENTED_EDGE ( 'NONE', *, *, #2179, .T. ) ;
#13599 = DIRECTION ( 'NONE',  ( 0.000000000000000000, 0.000000000000000000, 1.000000000000000000 ) ) ;
#13600 = VECTOR ( 'NONE', #13101, 1000.000000000000000 ) ;
#13601 = CARTESIAN_POINT ( 'NONE',  ( -8.635722793752535154, 94.60824746434937538, -19.90313979694426649 ) ) ;
#13602 = CARTESIAN_POINT ( 'NONE',  ( -0.3461262719736152849, 4.658553426539284281, -3.671615880910373608 ) ) ;
#13603 = CARTESIAN_POINT ( 'NONE',  ( 0.6666666666666655194, 4.233901974057256545, -3.300726591567080259 ) ) ;
#13604 = DIRECTION ( 'NONE',  ( 0.000000000000000000, 0.000000000000000000, 1.000000000000000000 ) ) ;
#13605 = ADVANCED_FACE ( 'NONE', ( #5608 ), #13662, .T. ) ;
#13606 = CYLINDRICAL_SURFACE ( 'NONE', #11263, 5.000000000000000888 ) ;
#13607 = CARTESIAN_POINT ( 'NONE',  ( 44.79355920668810853, 31.05588327715852159, -8.000000000000000000 ) ) ;
#13608 = CIRCLE ( 'NONE', #3429, 10.00000000000000355 ) ;
#13609 = ORIENTED_EDGE ( 'NONE', *, *, #7560, .F. ) ;
#13610 = LINE ( 'NONE', #10188, #10099 ) ;
#13611 = DIRECTION ( 'NONE',  ( 1.000000000000000000, 0.000000000000000000, 0.000000000000000000 ) ) ;
#13612 = AXIS2_PLACEMENT_3D ( 'NONE', #5863, #8295, #12934 ) ;
#13613 = CARTESIAN_POINT ( 'NONE',  ( 3.999999999999998224, 2.512223110932543690, -3.469391141908804599 ) ) ;
#13614 = B_SPLINE_CURVE_WITH_KNOTS ( 'NONE', 3,
 ( #4571, #3432, #9338, #1382, #11711, #7972, #12917, #2507 ),
 .UNSPECIFIED., .F., .F.,
 ( 4, 2, 2, 4 ),
 ( 0.000000000000000000, 0.002450665683189819696, 0.003675998524784729327, 0.004901331366379639391 ),
 .UNSPECIFIED. ) ;
#13615 = PRODUCT_DEFINITION_SHAPE ( 'NONE', 'NONE',  #15035 ) ;
#13616 = DIRECTION ( 'NONE',  ( 0.000000000000000000, 0.000000000000000000, -1.000000000000000000 ) ) ;
#13617 = ORIENTED_EDGE ( 'NONE', *, *, #9127, .F. ) ;
#13618 = DIRECTION ( 'NONE',  ( 0.000000000000000000, 0.000000000000000000, -1.000000000000000000 ) ) ;
#13619 = ORIENTED_EDGE ( 'NONE', *, *, #13447, .T. ) ;
#13620 = AXIS2_PLACEMENT_3D ( 'NONE', #13167, #2762, #11112 ) ;
#13621 = DIRECTION ( 'NONE',  ( 0.000000000000000000, 0.000000000000000000, 1.000000000000000000 ) ) ;
#13622 = DIRECTION ( 'NONE',  ( 1.000000000000000000, 0.000000000000000000, 0.000000000000000000 ) ) ;
#13623 = EDGE_LOOP ( 'NONE', ( #13736, #1596, #3489, #10936, #11464 ) ) ;
#13624 = EDGE_CURVE ( 'NONE', #10362, #13021, #14591, .T. ) ;
#13625 = CARTESIAN_POINT ( 'NONE',  ( 8.632958377326435340, 106.6512898904676092, -19.87266383408973525 ) ) ;
#13626 = EDGE_CURVE ( 'NONE', #12871, #2381, #9971, .T. ) ;
#13627 = AXIS2_PLACEMENT_3D ( 'NONE', #3338, #4629, #5828 ) ;
#13628 = CARTESIAN_POINT ( 'NONE',  ( 89.61631465359491244, 37.12029293941346708, -10.50000000000000000 ) ) ;
#13629 = ITEM_DEFINED_TRANSFORMATION ( 'NONE', 'NONE', #231,  #5108 ) ;
#13630 = VERTEX_POINT ( 'NONE', #6665 ) ;
#13631 = ORIENTED_EDGE ( 'NONE', *, *, #8649, .F. ) ;
#13632 = ORIENTED_EDGE ( 'NONE', *, *, #2965, .F. ) ;
#13633 = DIRECTION ( 'NONE',  ( 0.000000000000000000, 0.000000000000000000, 1.000000000000000000 ) ) ;
#13634 = CARTESIAN_POINT ( 'NONE',  ( 26.01438936481372721, 47.21331623427104063, -13.00000000000000178 ) ) ;
#13635 = CIRCLE ( 'NONE', #7324, 59.50000000000000000 ) ;
#13636 = DIRECTION ( 'NONE',  ( 1.000000000000000000, 0.000000000000000000, 0.000000000000000000 ) ) ;
#13637 = EDGE_LOOP ( 'NONE', ( #7951, #4952, #6782, #9868, #9713 ) ) ;
#13638 = EDGE_CURVE ( 'NONE', #3039, #6857, #5375, .T. ) ;
#13639 = MECHANICAL_DESIGN_GEOMETRIC_PRESENTATION_REPRESENTATION (  '', ( #796 ), #2241 ) ;
#13640 = ORIENTED_EDGE ( 'NONE', *, *, #1518, .F. ) ;
#13641 = ORIENTED_EDGE ( 'NONE', *, *, #3291, .F. ) ;
#13642 = DIRECTION ( 'NONE',  ( 0.000000000000000000, 0.000000000000000000, 1.000000000000000000 ) ) ;
#13643 = VECTOR ( 'NONE', #4173, 1000.000000000000000 ) ;
#13644 = AXIS2_PLACEMENT_3D ( 'NONE', #9714, #3670, #7216 ) ;
#13645 = CARTESIAN_POINT ( 'NONE',  ( -50.00000000000000000, 0.000000000000000000, 8.000000000000000000 ) ) ;
#13646 = EDGE_CURVE ( 'NONE', #11976, #11994, #10708, .T. ) ;
#13647 = CYLINDRICAL_SURFACE ( 'NONE', #77, 0.5000000000000073275 ) ;
#13648 =( NAMED_UNIT ( * ) SI_UNIT ( $, .STERADIAN. ) SOLID_ANGLE_UNIT ( ) );
#13649 = DIRECTION ( 'NONE',  ( -1.000000000000000000, 0.000000000000000000, 0.000000000000000000 ) ) ;
#13650 = VERTEX_POINT ( 'NONE', #10466 ) ;
#13651 = FACE_BOUND ( 'NONE', #9746, .T. ) ;
#13652 = DIRECTION ( 'NONE',  ( -1.000000000000000000, 0.000000000000000000, 0.000000000000000000 ) ) ;
#13653 = VERTEX_POINT ( 'NONE', #3188 ) ;
#13654 = FACE_OUTER_BOUND ( 'NONE', #2006, .T. ) ;
#13655 = AXIS2_PLACEMENT_3D ( 'NONE', #426, #14246, #4828 ) ;
#13656 = ORIENTED_EDGE ( 'NONE', *, *, #13821, .T. ) ;
#13657 = CIRCLE ( 'NONE', #9038, 3.000000000000002665 ) ;
#13658 = ORIENTED_EDGE ( 'NONE', *, *, #6905, .F. ) ;
#13659 = DIRECTION ( 'NONE',  ( -1.000000000000000000, 0.000000000000000000, 0.000000000000000000 ) ) ;
#13660 = ORIENTED_EDGE ( 'NONE', *, *, #3072, .F. ) ;
#13661 = CARTESIAN_POINT ( 'NONE',  ( 5.200000000000006395, 0.000000000000000000, 2.775557561562891351E-14 ) ) ;
#13662 = CYLINDRICAL_SURFACE ( 'NONE', #11450, 63.00000000000000000 ) ;
#13663 = CIRCLE ( 'NONE', #9529, 59.50000000000000000 ) ;
#13664 = CYLINDRICAL_SURFACE ( 'NONE', #7643, 0.5000000000000004441 ) ;
#13665 = CARTESIAN_POINT ( 'NONE',  ( 0.000000000000000000, 0.000000000000000000, 0.000000000000000000 ) ) ;
#13666 = B_SPLINE_CURVE_WITH_KNOTS ( 'NONE', 3,
 ( #11948, #11863, #9350, #3892, #12926, #2440, #8366, #8506, #397, #13153, #5030, #5856, #10493, #92, #323, #3667, #13998, #14141, #6075, #8210 ),
 .UNSPECIFIED., .F., .F.,
 ( 4, 2, 2, 2, 2, 2, 2, 2, 2, 4 ),
 ( 0.000000000000000000, 0.0009783709435495487137, 0.001467556415324328166, 0.001956741887099107836, 0.002935112830648676282, 0.003913483774198245162, 0.004891854717747813608, 0.005870225661297382054, 0.006848596604846951368, 0.007826967548396519814 ),
 .UNSPECIFIED. ) ;
#13667 = CARTESIAN_POINT ( 'NONE',  ( 0.000000000000000000, 0.000000000000000000, -8.000000000000000000 ) ) ;
#13668 = CIRCLE ( 'NONE', #13183, 50.00000000000000000 ) ;
#13669 = ORIENTED_EDGE ( 'NONE', *, *, #4618, .T. ) ;
#13670 = FACE_OUTER_BOUND ( 'NONE', #4582, .T. ) ;
#13671 = VERTEX_POINT ( 'NONE', #5758 ) ;
#13672 = EDGE_CURVE ( 'NONE', #10698, #14931, #10961, .T. ) ;
#13673 = AXIS2_PLACEMENT_3D ( 'NONE', #2750, #9499, #4889 ) ;
#13674 = DIRECTION ( 'NONE',  ( 1.000000000000000000, 0.000000000000000000, 0.000000000000000000 ) ) ;
#13675 = DIRECTION ( 'NONE',  ( -0.000000000000000000, -0.000000000000000000, -1.000000000000000000 ) ) ;
#13676 = EDGE_CURVE ( 'NONE', #4514, #469, #12418, .T. ) ;
#13677 = CIRCLE ( 'NONE', #3504, 57.00000000000000000 ) ;
#13678 = ORIENTED_EDGE ( 'NONE', *, *, #13873, .F. ) ;
#13679 = PLANE ( 'NONE',  #13221 ) ;
#13680 = CARTESIAN_POINT ( 'NONE',  ( 34.13789039812933623, 95.05637002121841306, 16.00000000000000711 ) ) ;
#13681 = CARTESIAN_POINT ( 'NONE',  ( 49.11971303961677648, 15.88467684210564990, 8.000000000000000000 ) ) ;
#13682 = FACE_OUTER_BOUND ( 'NONE', #11488, .T. ) ;
#13683 = CYLINDRICAL_SURFACE ( 'NONE', #14565, 0.5000000000000004441 ) ;
#13684 = CARTESIAN_POINT ( 'NONE',  ( 0.000000000000000000, 0.000000000000000000, -5.000000000000000888 ) ) ;
#13685 = TOROIDAL_SURFACE ( 'NONE', #4003, 17.00000000000001066, 5.000000000000000000 ) ;
#13686 = AXIS2_PLACEMENT_3D ( 'NONE', #3237, #11444, #1043 ) ;
#13687 = VECTOR ( 'NONE', #8923, 1000.000000000000000 ) ;
#13688 = DIRECTION ( 'NONE',  ( 1.000000000000000000, 0.000000000000000000, 0.000000000000000000 ) ) ;
#13689 = DIRECTION ( 'NONE',  ( -1.000000000000000000, 0.000000000000000000, 0.000000000000000000 ) ) ;
#13690 = EDGE_CURVE ( 'NONE', #8255, #2714, #4658, .T. ) ;
#13691 = ORIENTED_EDGE ( 'NONE', *, *, #5862, .T. ) ;
#13692 = CARTESIAN_POINT ( 'NONE',  ( -12.86891638962156215, 56.43380494353993271, 8.000000000000000000 ) ) ;
#13693 = VERTEX_POINT ( 'NONE', #14807 ) ;
#13694 = EDGE_CURVE ( 'NONE', #14215, #3803, #12756, .T. ) ;
#13695 = CARTESIAN_POINT ( 'NONE',  ( -31.95997502295763582, 41.65105036529000415, -10.50000000000000000 ) ) ;
#13696 = CARTESIAN_POINT ( 'NONE',  ( 9.449524216731116866, 94.52924706620449058, -19.61300924954587188 ) ) ;
#13697 = CIRCLE ( 'NONE', #1815, 0.5000000000000022204 ) ;
#13698 = DIRECTION ( 'NONE',  ( 1.000000000000000000, 0.000000000000000000, 0.000000000000000000 ) ) ;
#13699 = AXIS2_PLACEMENT_3D ( 'NONE', #10971, #6396, #4987 ) ;
#13700 = VECTOR ( 'NONE', #1634, 1000.000000000000000 ) ;
#13701 = AXIS2_PLACEMENT_3D ( 'NONE', #1344, #6023, #5955 ) ;
#13702 = CARTESIAN_POINT ( 'NONE',  ( 0.000000000000000000, 0.000000000000000000, -10.50000000000000000 ) ) ;
#13703 = ORIENTED_EDGE ( 'NONE', *, *, #5699, .T. ) ;
#13704 = CARTESIAN_POINT ( 'NONE',  ( 0.1756481739660548935, -4.720212674038995360, -3.469390959564072396 ) ) ;
#13705 = EDGE_LOOP ( 'NONE', ( #1045, #1947, #9641, #12932, #12592, #8288 ) ) ;
#13706 = DIRECTION ( 'NONE',  ( -1.000000000000000000, 0.000000000000000000, 0.000000000000000000 ) ) ;
#13707 = DIRECTION ( 'NONE',  ( 0.000000000000000000, 0.000000000000000000, 1.000000000000000000 ) ) ;
#13708 = ORIENTED_EDGE ( 'NONE', *, *, #14836, .F. ) ;
#13709 =( GEOMETRIC_REPRESENTATION_CONTEXT ( 3 ) GLOBAL_UNCERTAINTY_ASSIGNED_CONTEXT ( ( #14737 ) ) GLOBAL_UNIT_ASSIGNED_CONTEXT ( ( #3058, #1902, #14674 ) ) REPRESENTATION_CONTEXT ( 'NONE', 'WORKASPACE' ) );
#13710 = CARTESIAN_POINT ( 'NONE',  ( -68.58935777509570642, -68.58935777509452691, -13.00000000000000178 ) ) ;
#13711 = DIRECTION ( 'NONE',  ( -1.000000000000000000, 0.000000000000000000, 0.000000000000000000 ) ) ;
#13712 = ORIENTED_EDGE ( 'NONE', *, *, #1572, .T. ) ;
#13713 = CIRCLE ( 'NONE', #11413, 50.00000000000000000 ) ;
#13714 = VECTOR ( 'NONE', #5343, 1000.000000000000000 ) ;
#13715 = CIRCLE ( 'NONE', #10314, 3.000000000000002665 ) ;
#13716 = VERTEX_POINT ( 'NONE', #9019 ) ;
#13717 = ORIENTED_EDGE ( 'NONE', *, *, #7014, .F. ) ;
#13718 = ORIENTED_EDGE ( 'NONE', *, *, #11361, .F. ) ;
#13719 = CARTESIAN_POINT ( 'NONE',  ( -12.86891638962156215, 56.43380494353993271, -13.00000000000000178 ) ) ;
#13720 = CARTESIAN_POINT ( 'NONE',  ( 31.47058823529413729, 102.2673069760056563, 10.99999999999999645 ) ) ;
#13721 = DIRECTION ( 'NONE',  ( -0.2941176470588243164, -0.9557692240748185686, -0.000000000000000000 ) ) ;
#13722 = AXIS2_PLACEMENT_3D ( 'NONE', #9828, #12960, #2707 ) ;
#13723 = ORIENTED_EDGE ( 'NONE', *, *, #13125, .T. ) ;
#13724 = ADVANCED_FACE ( 'NONE', ( #2275 ), #12130, .F. ) ;
#13725 = CIRCLE ( 'NONE', #7154, 3.000000000000002665 ) ;
#13726 = EDGE_CURVE ( 'NONE', #2878, #14215, #14348, .T. ) ;
#13727 = ORIENTED_EDGE ( 'NONE', *, *, #2021, .T. ) ;
#13728 = ORIENTED_EDGE ( 'NONE', *, *, #6369, .T. ) ;
#13729 = DIRECTION ( 'NONE',  ( -1.000000000000000000, 0.000000000000000000, 0.000000000000000000 ) ) ;
#13730 = DIRECTION ( 'NONE',  ( 0.000000000000000000, 0.000000000000000000, -1.000000000000000000 ) ) ;
#13731 = CARTESIAN_POINT ( 'NONE',  ( -7.500000000000000888, 106.2673515243510991, 20.00000000000000000 ) ) ;
#13732 =( LENGTH_UNIT ( ) NAMED_UNIT ( * ) SI_UNIT ( .MILLI., .METRE. ) );
#13733 = CARTESIAN_POINT ( 'NONE',  ( -22.05882352941176450, 71.68269180561142662, -23.50000000000000000 ) ) ;
#13734 = AXIS2_PLACEMENT_3D ( 'NONE', #4002, #353, #2557 ) ;
#13735 = EDGE_CURVE ( 'NONE', #879, #4205, #6892, .T. ) ;
#13736 = ORIENTED_EDGE ( 'NONE', *, *, #12795, .T. ) ;
#13737 = CARTESIAN_POINT ( 'NONE',  ( -9.706953719245875689, -57.06275842387046993, -13.00000000000000178 ) ) ;
#13738 = ORIENTED_EDGE ( 'NONE', *, *, #11192, .T. ) ;
#13739 = DIRECTION ( 'NONE',  ( 0.000000000000000000, 0.000000000000000000, 1.000000000000000000 ) ) ;
#13740 = ORIENTED_EDGE ( 'NONE', *, *, #5595, .F. ) ;
#13741 = ORIENTED_EDGE ( 'NONE', *, *, #13254, .F. ) ;
#13742 = EDGE_CURVE ( 'NONE', #3199, #4159, #12906, .T. ) ;
#13743 = EDGE_CURVE ( 'NONE', #4485, #3890, #2230, .T. ) ;
#13744 = ORIENTED_EDGE ( 'NONE', *, *, #4587, .T. ) ;
#13745 = CARTESIAN_POINT ( 'NONE',  ( -3.999999999999996447, 2.309401076758498039, -3.433295621305378020 ) ) ;
#13746 = CIRCLE ( 'NONE', #649, 0.5000000000000004441 ) ;
#13747 = EDGE_LOOP ( 'NONE', ( #9503, #12199, #3154, #402, #9526, #7758 ) ) ;
#13748 = LINE ( 'NONE', #60, #8265 ) ;
#13749 = DIRECTION ( 'NONE',  ( 1.000000000000000000, 0.000000000000000000, 0.000000000000000000 ) ) ;
#13750 = DIRECTION ( 'NONE',  ( -0.000000000000000000, -0.000000000000000000, 1.000000000000000000 ) ) ;
#13751 = CARTESIAN_POINT ( 'NONE',  ( -1.243802165048849773, 3.900692638707412563, -3.223146290109620615 ) ) ;
#13752 = DIRECTION ( 'NONE',  ( 1.000000000000000000, 0.000000000000000000, -0.000000000000000000 ) ) ;
#13753 = VERTEX_POINT ( 'NONE', #8112 ) ;
#13754 = AXIS2_PLACEMENT_3D ( 'NONE', #11605, #11540, #9158 ) ;
#13755 = CIRCLE ( 'NONE', #8160, 3.000000000000002665 ) ;
#13756 = DIRECTION ( 'NONE',  ( 0.000000000000000000, 0.000000000000000000, 1.000000000000000000 ) ) ;
#13757 = ORIENTED_EDGE ( 'NONE', *, *, #4157, .T. ) ;
#13758 = CARTESIAN_POINT ( 'NONE',  ( 25.00000000000000000, 81.24038404635960831, -16.00000000000000000 ) ) ;
#13759 = DIRECTION ( 'NONE',  ( 1.000000000000000000, 0.000000000000000000, 0.000000000000000000 ) ) ;
#13760 = ORIENTED_EDGE ( 'NONE', *, *, #4455, .T. ) ;
#13761 = CARTESIAN_POINT ( 'NONE',  ( 39.66766701456161570, 30.43807145043622597, -8.000000000000000000 ) ) ;
#13762 = VERTEX_POINT ( 'NONE', #3412 ) ;
#13763 = DIRECTION ( 'NONE',  ( 0.000000000000000000, 0.000000000000000000, -1.000000000000000000 ) ) ;
#13764 = VERTEX_POINT ( 'NONE', #8941 ) ;
#13765 = CARTESIAN_POINT ( 'NONE',  ( 0.000000000000000000, 0.000000000000000000, -4.484454397937119197 ) ) ;
#13766 = CARTESIAN_POINT ( 'NONE',  ( -23.50071946824040836, -45.96504489226015977, -8.000000000000000000 ) ) ;
#13767 = DIRECTION ( 'NONE',  ( -1.000000000000000000, 0.000000000000000000, 0.000000000000000000 ) ) ;
#13768 = EDGE_CURVE ( 'NONE', #12241, #2474, #3492, .T. ) ;
#13769 = FACE_OUTER_BOUND ( 'NONE', #4556, .T. ) ;
#13770 = CARTESIAN_POINT ( 'NONE',  ( -3.999999999999998224, -0.8382240730041846666, -3.220610619767136473 ) ) ;
#13771 = DIRECTION ( 'NONE',  ( -0.000000000000000000, -0.000000000000000000, -1.000000000000000000 ) ) ;
#13772 = VERTEX_POINT ( 'NONE', #12976 ) ;
#13773 = DIRECTION ( 'NONE',  ( -0.000000000000000000, -0.000000000000000000, 1.000000000000000000 ) ) ;
#13774 = DIRECTION ( 'NONE',  ( 0.000000000000000000, 0.000000000000000000, -1.000000000000000000 ) ) ;
#13775 = CIRCLE ( 'NONE', #4792, 0.5000000000000043299 ) ;
#13776 = DIRECTION ( 'NONE',  ( 0.000000000000000000, 0.000000000000000000, 1.000000000000000000 ) ) ;
#13777 = DIRECTION ( 'NONE',  ( -0.000000000000000000, -0.000000000000000000, 1.000000000000000000 ) ) ;
#13778 = ORIENTED_EDGE ( 'NONE', *, *, #5157, .F. ) ;
#13779 = DIRECTION ( 'NONE',  ( 1.000000000000000000, 0.000000000000000000, 0.000000000000000000 ) ) ;
#13780 = ORIENTED_EDGE ( 'NONE', *, *, #8510, .T. ) ;
#13781 = EDGE_CURVE ( 'NONE', #5385, #7405, #9012, .T. ) ;
#13782 = DIRECTION ( 'NONE',  ( 1.000000000000000000, 0.000000000000000000, 0.000000000000000000 ) ) ;
#13783 = ADVANCED_FACE ( 'NONE', ( #1365 ), #14038, .F. ) ;
#13784 = CYLINDRICAL_SURFACE ( 'NONE', #12915, 0.5000000000000004441 ) ;
#13785 = EDGE_CURVE ( 'NONE', #143, #10570, #2592, .T. ) ;
#13786 = AXIS2_PLACEMENT_3D ( 'NONE', #7177, #14102, #5814 ) ;
#13787 = CARTESIAN_POINT ( 'NONE',  ( 5.000000000000007994, 0.000000000000000000, 2.775557561562891351E-14 ) ) ;
#13788 = DIRECTION ( 'NONE',  ( -1.000000000000000000, 0.000000000000000000, 0.000000000000000000 ) ) ;
#13789 = ORIENTED_EDGE ( 'NONE', *, *, #5315, .T. ) ;
#13790 = ORIENTED_EDGE ( 'NONE', *, *, #11705, .F. ) ;
#13791 = ORIENTED_EDGE ( 'NONE', *, *, #2481, .T. ) ;
#13792 = EDGE_CURVE ( 'NONE', #2920, #5532, #7557, .T. ) ;
#13793 = DIRECTION ( 'NONE',  ( 1.000000000000000000, 0.000000000000000000, 0.000000000000000000 ) ) ;
#13794 = DIRECTION ( 'NONE',  ( -0.000000000000000000, -0.000000000000000000, -1.000000000000000000 ) ) ;
#13795 = DIRECTION ( 'NONE',  ( -0.000000000000000000, -0.000000000000000000, -1.000000000000000000 ) ) ;
#13796 = ORIENTED_EDGE ( 'NONE', *, *, #8508, .T. ) ;
#13797 = VERTEX_POINT ( 'NONE', #6042 ) ;
#13798 = VERTEX_POINT ( 'NONE', #3568 ) ;
#13799 = CARTESIAN_POINT ( 'NONE',  ( 10.20278626552728873, 74.30320229487229255, 19.21617406370430103 ) ) ;
#13800 = CARTESIAN_POINT ( 'NONE',  ( 0.000000000000000000, 0.000000000000000000, 13.50000000000000533 ) ) ;
#13801 = DIRECTION ( 'NONE',  ( -0.000000000000000000, -0.000000000000000000, -1.000000000000000000 ) ) ;
#13802 = DIRECTION ( 'NONE',  ( -0.000000000000000000, -0.000000000000000000, 1.000000000000000000 ) ) ;
#13803 = ORIENTED_EDGE ( 'NONE', *, *, #3413, .F. ) ;
#13804 = CARTESIAN_POINT ( 'NONE',  ( -36.14014761921588104, 11.74264578624790190, -28.00000000000000000 ) ) ;
#13805 = EDGE_CURVE ( 'NONE', #12336, #14898, #10890, .T. ) ;
#13806 = EDGE_LOOP ( 'NONE', ( #370, #2108, #9949, #366, #11220, #11930, #4863, #4061, #8330, #5747, #6058 ) ) ;
#13807 = CARTESIAN_POINT ( 'NONE',  ( 0.000000000000000000, 0.000000000000000000, 16.00000000000000000 ) ) ;
#13808 = AXIS2_PLACEMENT_3D ( 'NONE', #769, #4191, #13511 ) ;
#13809 = DIRECTION ( 'NONE',  ( 0.000000000000000000, 0.000000000000000000, 1.000000000000000000 ) ) ;
#13810 = ADVANCED_FACE ( 'NONE', ( #9391 ), #8610, .F. ) ;
#13811 = VERTEX_POINT ( 'NONE', #1789 ) ;
#13812 = ORIENTED_EDGE ( 'NONE', *, *, #12526, .T. ) ;
#13813 = CARTESIAN_POINT ( 'NONE',  ( 24.98583958711423492, -30.74264578624780597, 14.49999999999999822 ) ) ;
#13814 = ORIENTED_EDGE ( 'NONE', *, *, #10237, .T. ) ;
#13815 = ORIENTED_EDGE ( 'NONE', *, *, #4343, .T. ) ;
#13816 = DIRECTION ( 'NONE',  ( 1.000000000000000000, 0.000000000000000000, 0.000000000000000000 ) ) ;
#13817 = VECTOR ( 'NONE', #9765, 1000.000000000000000 ) ;
#13818 = DIRECTION ( 'NONE',  ( 1.000000000000000000, 1.826024711554534012E-15, 0.000000000000000000 ) ) ;
#13819 = LINE ( 'NONE', #12823, #5472 ) ;
#13820 = FACE_OUTER_BOUND ( 'NONE', #10229, .T. ) ;
#13821 = EDGE_CURVE ( 'NONE', #2546, #2335, #4181, .T. ) ;
#13822 = DIRECTION ( 'NONE',  ( 0.000000000000000000, 0.000000000000000000, 1.000000000000000000 ) ) ;
#13823 = EDGE_CURVE ( 'NONE', #4604, #9310, #13143, .T. ) ;
#13824 = ORIENTED_EDGE ( 'NONE', *, *, #14225, .T. ) ;
#13825 = SURFACE_STYLE_FILL_AREA ( #5342 ) ;
#13826 = AXIS2_PLACEMENT_3D ( 'NONE', #8958, #14903, #7744 ) ;
#13827 = AXIS2_PLACEMENT_3D ( 'NONE', #13787, #1864, #1929 ) ;
#13828 = VECTOR ( 'NONE', #14008, 1000.000000000000000 ) ;
#13829 = CARTESIAN_POINT ( 'NONE',  ( -51.45950017607691507, 4.121772567811807342, 8.000000000000000000 ) ) ;
#13830 = CIRCLE ( 'NONE', #977, 50.00000000000000000 ) ;
#13831 = ORIENTED_EDGE ( 'NONE', *, *, #4347, .T. ) ;
#13832 = CARTESIAN_POINT ( 'NONE',  ( -57.06275842387042729, 9.706953719246069312, -13.00000000000000178 ) ) ;
#13833 = EDGE_CURVE ( 'NONE', #12431, #1277, #11840, .T. ) ;
#13834 = EDGE_LOOP ( 'NONE', ( #8785, #4776, #6218, #4986, #3344, #396, #7181, #12677, #14218 ) ) ;
#13835 = CARTESIAN_POINT ( 'NONE',  ( 29.82779671029265245, 96.49509599019864936, 12.13403317654897329 ) ) ;
#13836 = CARTESIAN_POINT ( 'NONE',  ( -8.633615064400526506, 62.40799623593410672, 19.90332611805893137 ) ) ;
#13837 = AXIS2_PLACEMENT_3D ( 'NONE', #7203, #14129, #6213 ) ;
#13838 = CYLINDRICAL_SURFACE ( 'NONE', #10788, 63.00000000000000000 ) ;
#13840 = CARTESIAN_POINT ( 'NONE',  ( -9.706953719245875689, -57.06275842387046993, -10.50000000000000000 ) ) ;
#13839 = CIRCLE ( 'NONE', #4857, 59.50000000000000000 ) ;
#13841 = DIRECTION ( 'NONE',  ( -0.000000000000000000, -0.000000000000000000, -1.000000000000000000 ) ) ;
#13842 = AXIS2_PLACEMENT_3D ( 'NONE', #11856, #9004, #12230 ) ;
#13843 = DIRECTION ( 'NONE',  ( -0.000000000000000000, -0.000000000000000000, 1.000000000000000000 ) ) ;
#13844 = ADVANCED_FACE ( 'NONE', ( #7542 ), #9741, .T. ) ;
#13845 = PRESENTATION_LAYER_ASSIGNMENT (  '', '', ( #5347 ) ) ;
#13846 = CARTESIAN_POINT ( 'NONE',  ( 5.204748896376250896E-15, 85.00000000000000000, 46.00000000000000000 ) ) ;
#13847 = ORIENTED_EDGE ( 'NONE', *, *, #6799, .F. ) ;
#13848 = AXIS2_PLACEMENT_3D ( 'NONE', #7211, #3820, #3962 ) ;
#13849 = CARTESIAN_POINT ( 'NONE',  ( 7.252293700257532727, 53.06332297728244640, -10.50000000000000000 ) ) ;
#13850 = DIRECTION ( 'NONE',  ( 1.000000000000000000, 0.000000000000000000, 0.000000000000000000 ) ) ;
#13851 = CIRCLE ( 'NONE', #9229, 63.00000000000000000 ) ;
#13852 = DIRECTION ( 'NONE',  ( -0.2941176470588241498, -0.9557692240748186796, 0.000000000000000000 ) ) ;
#13853 = AXIS2_PLACEMENT_3D ( 'NONE', #8766, #1792, #13403 ) ;
#13854 = CARTESIAN_POINT ( 'NONE',  ( 49.00442420935993226, -30.80502811811213704, 8.000000000000000000 ) ) ;
#13855 = AXIS2_PLACEMENT_3D ( 'NONE', #6314, #7619, #1785 ) ;
#13856 = VERTEX_POINT ( 'NONE', #4778 ) ;
#13857 = FACE_OUTER_BOUND ( 'NONE', #4938, .T. ) ;
#13858 = EDGE_LOOP ( 'NONE', ( #6772, #14872, #11387, #5679 ) ) ;
#13859 = CARTESIAN_POINT ( 'NONE',  ( 22.33583958711425055, -30.74264578624780597, -25.50000000000000355 ) ) ;
#13860 = DIRECTION ( 'NONE',  ( 1.000000000000000000, 0.000000000000000000, -0.000000000000000000 ) ) ;
#13861 = AXIS2_PLACEMENT_3D ( 'NONE', #4094, #8703, #11077 ) ;
#13862 = DIRECTION ( 'NONE',  ( 0.000000000000000000, 0.000000000000000000, 1.000000000000000000 ) ) ;
#13863 = DIRECTION ( 'NONE',  ( -1.000000000000000000, 0.000000000000000000, 0.000000000000000000 ) ) ;
#13864 = VERTEX_POINT ( 'NONE', #13258 ) ;
#13865 = VECTOR ( 'NONE', #6946, 1000.000000000000000 ) ;
#13866 = ORIENTED_EDGE ( 'NONE', *, *, #8427, .F. ) ;
#13867 = AXIS2_PLACEMENT_3D ( 'NONE', #11621, #7887, #1146 ) ;
#13868 = ADVANCED_FACE ( 'NONE', ( #12115 ), #2850, .F. ) ;
#13869 = CARTESIAN_POINT ( 'NONE',  ( -12.07479981346993902, 61.83277384271320187, -17.09860361742227397 ) ) ;
#13870 = CARTESIAN_POINT ( 'NONE',  ( 45.88839665196118744, -26.99988008862642630, -13.00000000000000178 ) ) ;
#13871 = APPLICATION_CONTEXT ( 'automotive_design' ) ;
#13872 = FACE_OUTER_BOUND ( 'NONE', #7987, .T. ) ;
#13873 = EDGE_CURVE ( 'NONE', #12602, #5519, #289, .T. ) ;
#13874 = EDGE_LOOP ( 'NONE', ( #8770, #1187, #5036, #11598, #3384, #5116, #3443, #3228, #6858, #6020 ) ) ;
#13875 = EDGE_CURVE ( 'NONE', #5875, #7688, #5205, .T. ) ;
#13876 = AXIS2_PLACEMENT_3D ( 'NONE', #167, #6917, #11794 ) ;
#13877 = VERTEX_POINT ( 'NONE', #13975 ) ;
#13878 = EDGE_LOOP ( 'NONE', ( #11165, #158, #6187, #14188, #4086 ) ) ;
#13879 = AXIS2_PLACEMENT_3D ( 'NONE', #7771, #14849, #11281 ) ;
#13880 = CARTESIAN_POINT ( 'NONE',  ( 10.88080562889580705, 74.20685544768620900, 18.69467976711750978 ) ) ;
#13881 = ADVANCED_FACE ( 'NONE', ( #1287 ), #5901, .F. ) ;
#13882 = DIRECTION ( 'NONE',  ( 1.000000000000000000, 0.000000000000000000, 0.000000000000000000 ) ) ;
#13883 = CARTESIAN_POINT ( 'NONE',  ( 68.09867107462983427, 68.49330278050145182, -10.50000000000000000 ) ) ;
#13884 = DIRECTION ( 'NONE',  ( -1.000000000000000000, -6.833935844856531060E-14, 0.000000000000000000 ) ) ;
#13885 = VECTOR ( 'NONE', #6072, 1000.000000000000000 ) ;
#13886 = FACE_OUTER_BOUND ( 'NONE', #12346, .T. ) ;
#13887 = ORIENTED_EDGE ( 'NONE', *, *, #937, .T. ) ;
#13888 = ADVANCED_FACE ( 'NONE', ( #5432 ), #12414, .F. ) ;
#13889 = EDGE_LOOP ( 'NONE', ( #267, #9329, #10366, #8618, #14290, #958, #891, #1983, #6757 ) ) ;
#13890 = CARTESIAN_POINT ( 'NONE',  ( 3.999999999999995559, 2.309401076758498039, -3.504271511727123922 ) ) ;
#13891 = DIRECTION ( 'NONE',  ( 0.000000000000000000, 0.000000000000000000, -1.000000000000000000 ) ) ;
#13892 = CIRCLE ( 'NONE', #14128, 59.50000000000000000 ) ;
#13893 = ADVANCED_FACE ( 'NONE', ( #4303 ), #12566, .T. ) ;
#13894 = EDGE_LOOP ( 'NONE', ( #3651, #8928 ) ) ;
#13895 = EDGE_LOOP ( 'NONE', ( #4983, #5300, #6453, #8863, #8559, #13100 ) ) ;
#13896 = LINE ( 'NONE', #1143, #2324 ) ;
#13897 = EDGE_LOOP ( 'NONE', ( #2209, #1989, #6252, #9129 ) ) ;
#13898 = CIRCLE ( 'NONE', #2248, 59.50000000000000000 ) ;
#13899 = DIRECTION ( 'NONE',  ( 0.000000000000000000, 0.000000000000000000, 1.000000000000000000 ) ) ;
#13900 = DIRECTION ( 'NONE',  ( -0.000000000000000000, -0.000000000000000000, 1.000000000000000000 ) ) ;
#13901 = AXIS2_PLACEMENT_3D ( 'NONE', #7605, #13462, #1992 ) ;
#13902 = DIRECTION ( 'NONE',  ( 1.000000000000000000, 0.000000000000000000, 0.000000000000000000 ) ) ;
#13903 = CARTESIAN_POINT ( 'NONE',  ( -4.175648173966052923, 2.207990556236527180, -3.469390959564063071 ) ) ;
#13904 = DIRECTION ( 'NONE',  ( -1.000000000000000000, 0.000000000000000000, 0.000000000000000000 ) ) ;
#13905 = VERTEX_POINT ( 'NONE', #4146 ) ;
#13906 = DIRECTION ( 'NONE',  ( 0.000000000000000000, 0.000000000000000000, 1.000000000000000000 ) ) ;
#13907 = ORIENTED_EDGE ( 'NONE', *, *, #506, .T. ) ;
#13908 = CIRCLE ( 'NONE', #7335, 56.99999999999999289 ) ;
#13909 = CARTESIAN_POINT ( 'NONE',  ( 70.20695371924547601, 57.06275842387054098, 10.49999999999999822 ) ) ;
#13910 = AXIS2_PLACEMENT_3D ( 'NONE', #4803, #5857, #2441 ) ;
#13911 = ORIENTED_EDGE ( 'NONE', *, *, #13061, .F. ) ;
#13912 = CARTESIAN_POINT ( 'NONE',  ( -33.48561063518626923, 47.21331623427104063, -13.00000000000000178 ) ) ;
#13913 = ORIENTED_EDGE ( 'NONE', *, *, #7260, .T. ) ;
#13914 = EDGE_CURVE ( 'NONE', #12897, #11572, #8763, .T. ) ;
#13915 = AXIS2_PLACEMENT_3D ( 'NONE', #8539, #8615, #13185 ) ;
#13916 = CARTESIAN_POINT ( 'NONE',  ( 31.56034153936680653, 95.94279256428042402, 14.97248702055886582 ) ) ;
#13917 = EDGE_CURVE ( 'NONE', #1935, #3975, #2008, .T. ) ;
#13918 = DIRECTION ( 'NONE',  ( 0.000000000000000000, 0.000000000000000000, 1.000000000000000000 ) ) ;
#13919 = EDGE_CURVE ( 'NONE', #14223, #4677, #14601, .T. ) ;
#13920 = CARTESIAN_POINT ( 'NONE',  ( 3.999999999999996447, 2.309401076758511806, -0.5000000000000004441 ) ) ;
#13921 = CARTESIAN_POINT ( 'NONE',  ( -11.99124924651179924, 106.3260354126052079, 17.22144562113021138 ) ) ;
#13922 = LINE ( 'NONE', #3513, #12856 ) ;
#13923 = CARTESIAN_POINT ( 'NONE',  ( -3.999999999999998224, 1.677772373332607092, -3.535253723896766509 ) ) ;
#13924 = SHAPE_DEFINITION_REPRESENTATION ( #7533, #1232 ) ;
#13925 = EDGE_CURVE ( 'NONE', #14497, #7611, #9983, .T. ) ;
#13926 = DIRECTION ( 'NONE',  ( 1.000000000000000000, 0.000000000000000000, 0.000000000000000000 ) ) ;
#13927 = CIRCLE ( 'NONE', #3732, 52.50000000000000711 ) ;
#13928 = ORIENTED_EDGE ( 'NONE', *, *, #3523, .F. ) ;
#13929 = DIRECTION ( 'NONE',  ( 1.000000000000000000, 0.000000000000000000, 0.000000000000000000 ) ) ;
#13930 = DIRECTION ( 'NONE',  ( 0.000000000000000000, 0.000000000000000000, 1.000000000000000000 ) ) ;
#13931 = FACE_OUTER_BOUND ( 'NONE', #7086, .T. ) ;
#13932 = CARTESIAN_POINT ( 'NONE',  ( 0.000000000000000000, 0.000000000000000000, -13.00000000000000178 ) ) ;
#13933 = EDGE_CURVE ( 'NONE', #6415, #11737, #8291, .T. ) ;
#13934 = ORIENTED_EDGE ( 'NONE', *, *, #15003, .F. ) ;
#13935 = AXIS2_PLACEMENT_3D ( 'NONE', #10107, #5406, #12317 ) ;
#13936 = AXIS2_PLACEMENT_3D ( 'NONE', #12437, #6648, #3099 ) ;
#13937 = DIRECTION ( 'NONE',  ( 1.000000000000000000, 0.000000000000000000, 0.000000000000000000 ) ) ;
#13938 = AXIS2_PLACEMENT_3D ( 'NONE', #11810, #11734, #13091 ) ;
#13939 = ORIENTED_EDGE ( 'NONE', *, *, #5049, .F. ) ;
#13940 = CARTESIAN_POINT ( 'NONE',  ( -2.000000000000008882, 3.464101615137750390, 0.000000000000000000 ) ) ;
#13941 = DIRECTION ( 'NONE',  ( 0.000000000000000000, 0.000000000000000000, -1.000000000000000000 ) ) ;
#13942 = CARTESIAN_POINT ( 'NONE',  ( 31.05588327715836527, -44.79355920668822932, -13.00000000000000178 ) ) ;
#13943 = DIRECTION ( 'NONE',  ( -0.000000000000000000, -0.000000000000000000, -1.000000000000000000 ) ) ;
#13944 = EDGE_LOOP ( 'NONE', ( #2458, #7558, #10353, #10906, #1105 ) ) ;
#13945 = ORIENTED_EDGE ( 'NONE', *, *, #6638, .F. ) ;
#13946 = CIRCLE ( 'NONE', #4256, 3.000000000000002665 ) ;
#13947 = CARTESIAN_POINT ( 'NONE',  ( 92.38795325112877777, 38.26834323650874126, 8.000000000000000000 ) ) ;
#13948 = CARTESIAN_POINT ( 'NONE',  ( -44.89637028918152595, 0.000000000000000000, -25.50000000000000355 ) ) ;
#13949 = AXIS2_PLACEMENT_3D ( 'NONE', #746, #4245, #4168 ) ;
#13950 = CARTESIAN_POINT ( 'NONE',  ( 41.59008834022645829, 32.46576781417968505, -13.00000000000000178 ) ) ;
#13951 = EDGE_LOOP ( 'NONE', ( #5201, #13255, #1784, #13907, #4249 ) ) ;
#13952 = ORIENTED_EDGE ( 'NONE', *, *, #8373, .T. ) ;
#13953 = AXIS2_PLACEMENT_3D ( 'NONE', #878, #950, #2002 ) ;
#13954 = ORIENTED_EDGE ( 'NONE', *, *, #9405, .F. ) ;
#13955 = AXIS2_PLACEMENT_3D ( 'NONE', #6104, #5127, #9740 ) ;
#13956 = CARTESIAN_POINT ( 'NONE',  ( 51.19406879332056093, 13.71740939043382745, -13.00000000000000178 ) ) ;
#13957 = AXIS2_PLACEMENT_3D ( 'NONE', #9340, #1090, #4793 ) ;
#13958 = DIRECTION ( 'NONE',  ( -0.000000000000000000, -0.000000000000000000, -1.000000000000000000 ) ) ;
#13959 = CARTESIAN_POINT ( 'NONE',  ( 4.235886605889390921, 2.417314728048529204, -3.751161874094020465 ) ) ;
#13960 = EDGE_CURVE ( 'NONE', #13160, #1886, #5624, .T. ) ;
#13961 = DIRECTION ( 'NONE',  ( -0.000000000000000000, -0.000000000000000000, 1.000000000000000000 ) ) ;
#13962 = EDGE_CURVE ( 'NONE', #6859, #12263, #2715, .T. ) ;
#13963 = CARTESIAN_POINT ( 'NONE',  ( 4.101954839143200360, -2.368264730583031774, -3.681130640444377988 ) ) ;
#13964 = ORIENTED_EDGE ( 'NONE', *, *, #10747, .F. ) ;
#13965 = DIRECTION ( 'NONE',  ( 1.000000000000000000, -1.243449787580175325E-14, 0.000000000000000000 ) ) ;
#13966 = DIRECTION ( 'NONE',  ( 1.000000000000000000, 0.000000000000000000, 0.000000000000000000 ) ) ;
#13967 = AXIS2_PLACEMENT_3D ( 'NONE', #12028, #6223, #10865 ) ;
#13968 = ORIENTED_EDGE ( 'NONE', *, *, #10753, .T. ) ;
#13969 = ORIENTED_EDGE ( 'NONE', *, *, #7548, .F. ) ;
#13970 = CARTESIAN_POINT ( 'NONE',  ( -86.67575032682103142, -37.71449950291016506, 8.000000000000000000 ) ) ;
#13971 = EDGE_LOOP ( 'NONE', ( #12091, #11674, #780, #11805 ) ) ;
#13972 = ORIENTED_EDGE ( 'NONE', *, *, #642, .T. ) ;
#13973 = CIRCLE ( 'NONE', #6674, 59.49999999999999289 ) ;
#13974 = CARTESIAN_POINT ( 'NONE',  ( -31.47058823529412663, 102.2673069760056421, 25.99999999999999645 ) ) ;
#13975 = CARTESIAN_POINT ( 'NONE',  ( 20.00000000000000000, 2.449293598294706513E-15, -28.00000000000000000 ) ) ;
#13976 = TOROIDAL_SURFACE ( 'NONE', #2073, 68.00000000000000000, 5.000000000000000000 ) ;
#13977 = CARTESIAN_POINT ( 'NONE',  ( -7.499999999999996447, 85.00000000000000000, 46.00000000000000000 ) ) ;
#13978 = DIRECTION ( 'NONE',  ( 0.000000000000000000, 0.000000000000000000, 1.000000000000000000 ) ) ;
#13979 = ADVANCED_FACE ( 'NONE', ( #8985 ), #886, .F. ) ;
#13980 = EDGE_CURVE ( 'NONE', #877, #11546, #9497, .T. ) ;
#13981 = CARTESIAN_POINT ( 'NONE',  ( 34.48472847331528612, 95.06210339626261430, -10.99999999999999645 ) ) ;
#13982 = CARTESIAN_POINT ( 'NONE',  ( -19.68583958711381854, -30.74264578624812927, -28.00000000000000000 ) ) ;
#13983 = VERTEX_POINT ( 'NONE', #10126 ) ;
#13984 = DIRECTION ( 'NONE',  ( 1.000000000000000000, 0.000000000000000000, 0.000000000000000000 ) ) ;
#13985 = ORIENTED_EDGE ( 'NONE', *, *, #4157, .F. ) ;
#13986 = CYLINDRICAL_SURFACE ( 'NONE', #3056, 63.00000000000000000 ) ;
#13987 = ORIENTED_EDGE ( 'NONE', *, *, #441, .F. ) ;
#13988 = CARTESIAN_POINT ( 'NONE',  ( 29.86558579037015804, 96.48341332593348341, 12.29240575635729193 ) ) ;
#13989 = DIRECTION ( 'NONE',  ( 1.000000000000000000, 0.000000000000000000, 0.000000000000000000 ) ) ;
#13990 = CARTESIAN_POINT ( 'NONE',  ( 3.679171394226030234, 2.494631558665830529, -0.3503314178412461621 ) ) ;
#13991 = CARTESIAN_POINT ( 'NONE',  ( 0.000000000000000000, 4.862606272033088928, -3.745885042887437510 ) ) ;
#13992 = PLANE ( 'NONE',  #9209 ) ;
#13993 = CIRCLE ( 'NONE', #3322, 3.000000000000002665 ) ;
#13994 = DIRECTION ( 'NONE',  ( 0.000000000000000000, 0.000000000000000000, 1.000000000000000000 ) ) ;
#13995 = CARTESIAN_POINT ( 'NONE',  ( -22.33583958711380646, -30.74264578624812927, -25.50000000000000355 ) ) ;
#13996 = VERTEX_POINT ( 'NONE', #1863 ) ;
#13997 = EDGE_CURVE ( 'NONE', #6857, #9553, #12496, .T. ) ;
#13998 = CARTESIAN_POINT ( 'NONE',  ( -8.801203450618842794, 106.6379082728991676, -19.83890680725670919 ) ) ;
#13999 = LINE ( 'NONE', #10415, #10522 ) ;
#14000 = ADVANCED_FACE ( 'NONE', ( #7622 ), #4908, .T. ) ;
#14001 = CARTESIAN_POINT ( 'NONE',  ( 0.000000000000000000, 0.000000000000000000, -10.50000000000000000 ) ) ;
#14002 = CARTESIAN_POINT ( 'NONE',  ( 97.00000000000000000, -3.384287605079545030E-13, -8.000000000000000000 ) ) ;
#14003 = ORIENTED_EDGE ( 'NONE', *, *, #6210, .T. ) ;
#14004 = EDGE_CURVE ( 'NONE', #5446, #12855, #2959, .T. ) ;
#14005 = DIRECTION ( 'NONE',  ( 1.000000000000000000, 0.000000000000000000, 0.000000000000000000 ) ) ;
#14006 = MANIFOLD_SOLID_BREP ( 'M5 Clearance Hole1', #434 ) ;
#14007 = EDGE_LOOP ( 'NONE', ( #10642, #6878, #10876, #761, #15027, #3318 ) ) ;
#14008 = DIRECTION ( 'NONE',  ( 0.000000000000000000, -1.000000000000000000, 0.000000000000000000 ) ) ;
#14009 = CARTESIAN_POINT ( 'NONE',  ( -89.61631465359441506, 37.12029293941468211, -13.00000000000000178 ) ) ;
#14010 = LINE ( 'NONE', #13942, #732 ) ;
#14011 = DIRECTION ( 'NONE',  ( 0.000000000000000000, 0.000000000000000000, 1.000000000000000000 ) ) ;
#14012 = EDGE_CURVE ( 'NONE', #14795, #6680, #1997, .T. ) ;
#14013 = ORIENTED_EDGE ( 'NONE', *, *, #10283, .T. ) ;
#14014 = EDGE_CURVE ( 'NONE', #7044, #1401, #8076, .T. ) ;
#14015 = LINE ( 'NONE', #4819, #5249 ) ;
#14016 = DIRECTION ( 'NONE',  ( -0.000000000000000000, -0.000000000000000000, 1.000000000000000000 ) ) ;
#14017 = DIRECTION ( 'NONE',  ( 0.000000000000000000, 0.000000000000000000, -1.000000000000000000 ) ) ;
#14018 = ORIENTED_EDGE ( 'NONE', *, *, #2376, .T. ) ;
#14019 = ORIENTED_EDGE ( 'NONE', *, *, #14320, .F. ) ;
#14020 = ADVANCED_FACE ( 'NONE', ( #9424 ), #3679, .T. ) ;
#14021 = VERTEX_POINT ( 'NONE', #1109 ) ;
#14022 = DIRECTION ( 'NONE',  ( 1.000000000000000000, 0.000000000000000000, 0.000000000000000000 ) ) ;
#14023 = CARTESIAN_POINT ( 'NONE',  ( 89.61631465359491244, 37.12029293941346708, 8.000000000000000000 ) ) ;
#14024 = CARTESIAN_POINT ( 'NONE',  ( 5.200000000000006395, 3.306546357697854226E-16, 2.700000000000028155 ) ) ;
#14025 = DIRECTION ( 'NONE',  ( 1.000000000000000000, 0.000000000000000000, 0.000000000000000000 ) ) ;
#14026 = DIRECTION ( 'NONE',  ( 0.000000000000000000, 0.000000000000000000, 1.000000000000000000 ) ) ;
#14027 = CARTESIAN_POINT ( 'NONE',  ( -8.636355552181207429, 94.60704768011227372, 19.87755835258713333 ) ) ;
#14028 = ORIENTED_EDGE ( 'NONE', *, *, #13259, .F. ) ;
#14029 = ORIENTED_EDGE ( 'NONE', *, *, #11977, .F. ) ;
#14030 = DIRECTION ( 'NONE',  ( 1.000000000000000000, 0.000000000000000000, 0.000000000000000000 ) ) ;
#14031 = DIRECTION ( 'NONE',  ( 0.000000000000000000, 0.000000000000000000, -1.000000000000000000 ) ) ;
#14032 = DIRECTION ( 'NONE',  ( 0.000000000000000000, 0.000000000000000000, -1.000000000000000000 ) ) ;
#14033 = ORIENTED_EDGE ( 'NONE', *, *, #5983, .T. ) ;
#14034 = EDGE_LOOP ( 'NONE', ( #975, #11632, #5161, #14544, #7003 ) ) ;
#14035 = DIRECTION ( 'NONE',  ( -1.000000000000000000, 0.000000000000000000, 0.000000000000000000 ) ) ;
#14036 = EDGE_LOOP ( 'NONE', ( #14490, #11860, #9436, #10965, #5058 ) ) ;
#14037 = CARTESIAN_POINT ( 'NONE',  ( 24.99999999999975131, 43.30127018922208038, -8.000000000000000000 ) ) ;
#14038 = PLANE ( 'NONE',  #45 ) ;
#14039 = CARTESIAN_POINT ( 'NONE',  ( 0.000000000000000000, 0.000000000000000000, -10.50000000000000000 ) ) ;
#14040 = DIRECTION ( 'NONE',  ( -1.000000000000000000, -1.953992523340275511E-14, 0.000000000000000000 ) ) ;
#14041 = ORIENTED_EDGE ( 'NONE', *, *, #2993, .F. ) ;
#14042 = DIRECTION ( 'NONE',  ( 0.000000000000000000, 0.000000000000000000, -1.000000000000000000 ) ) ;
#14043 = LINE ( 'NONE', #12826, #7493 ) ;
#14044 = ORIENTED_EDGE ( 'NONE', *, *, #7073, .F. ) ;
#14045 = SURFACE_SIDE_STYLE ('',( #13825 ) ) ;
#14046 = ADVANCED_FACE ( 'NONE', ( #5788 ), #12858, .T. ) ;
#14047 = ADVANCED_FACE ( 'NONE', ( #14074 ), #12790, .T. ) ;
#14048 = ORIENTED_EDGE ( 'NONE', *, *, #14856, .T. ) ;
#14049 = DIRECTION ( 'NONE',  ( -0.000000000000000000, -0.000000000000000000, 1.000000000000000000 ) ) ;
#14050 = EDGE_CURVE ( 'NONE', #3450, #4822, #11950, .T. ) ;
#14051 = EDGE_CURVE ( 'NONE', #5002, #13650, #10734, .T. ) ;
#14052 = ORIENTED_EDGE ( 'NONE', *, *, #9676, .T. ) ;
#14053 = AXIS2_PLACEMENT_3D ( 'NONE', #10487, #10267, #2364 ) ;
#14054 = FACE_OUTER_BOUND ( 'NONE', #10317, .T. ) ;
#14055 = DIRECTION ( 'NONE',  ( 1.000000000000000000, 0.000000000000000000, 0.000000000000000000 ) ) ;
#14056 = CYLINDRICAL_SURFACE ( 'NONE', #863, 7.500000000000001776 ) ;
#14057 = DIRECTION ( 'NONE',  ( 0.000000000000000000, 0.000000000000000000, 1.000000000000000000 ) ) ;
#14058 = CARTESIAN_POINT ( 'NONE',  ( 7.500000000000000000, 62.55197838597913318, 20.00000000000000000 ) ) ;
#14059 = AXIS2_PLACEMENT_3D ( 'NONE', #8840, #13405, #10975 ) ;
#14060 = DIRECTION ( 'NONE',  ( 0.000000000000000000, 0.000000000000000000, 1.000000000000000000 ) ) ;
#14061 = CARTESIAN_POINT ( 'NONE',  ( 12.50000000000000000, 106.2673515243510991, 15.00000000000000000 ) ) ;
#14062 = VERTEX_POINT ( 'NONE', #4813 ) ;
#14063 = AXIS2_PLACEMENT_3D ( 'NONE', #9778, #11011, #11162 ) ;
#14064 = CARTESIAN_POINT ( 'NONE',  ( 2.000000000000008882, 3.464101615137750390, 0.000000000000000000 ) ) ;
#14065 = CARTESIAN_POINT ( 'NONE',  ( -89.89283556784485540, 37.53686968382331202, -10.50000000000000000 ) ) ;
#14066 = DIRECTION ( 'NONE',  ( 0.000000000000000000, 0.000000000000000000, 1.000000000000000000 ) ) ;
#14067 = ADVANCED_FACE ( 'NONE', ( #3370 ), #2239, .F. ) ;
#14068 = DIRECTION ( 'NONE',  ( 0.000000000000000000, 0.000000000000000000, -1.000000000000000000 ) ) ;
#14069 = EDGE_LOOP ( 'NONE', ( #10658, #9952, #2367, #4405, #9685, #12844, #1764, #13945 ) ) ;
#14070 = FACE_OUTER_BOUND ( 'NONE', #9014, .T. ) ;
#14071 = ORIENTED_EDGE ( 'NONE', *, *, #2642, .T. ) ;
#14072 =( GEOMETRIC_REPRESENTATION_CONTEXT ( 3 ) GLOBAL_UNCERTAINTY_ASSIGNED_CONTEXT ( ( #6389 ) ) GLOBAL_UNIT_ASSIGNED_CONTEXT ( ( #675, #3026, #7713 ) ) REPRESENTATION_CONTEXT ( 'NONE', 'WORKASPACE' ) );
#14073 = DIRECTION ( 'NONE',  ( 1.000000000000000000, 0.000000000000000000, 0.000000000000000000 ) ) ;
#14074 = FACE_OUTER_BOUND ( 'NONE', #6865, .T. ) ;
#14075 = DIRECTION ( 'NONE',  ( -0.000000000000000000, -0.000000000000000000, -1.000000000000000000 ) ) ;
#14076 = CARTESIAN_POINT ( 'NONE',  ( 6.526309611002943711, 49.57224306869047581, 8.000000000000000000 ) ) ;
#14077 = VECTOR ( 'NONE', #13918, 1000.000000000000000 ) ;
#14078 = ORIENTED_EDGE ( 'NONE', *, *, #9493, .T. ) ;
#14079 = CARTESIAN_POINT ( 'NONE',  ( -12.50000000000000000, 106.2673515243510991, 15.00000000000000000 ) ) ;
#14080 = AXIS2_PLACEMENT_3D ( 'NONE', #6913, #4949, #6066 ) ;
#14081 = LINE ( 'NONE', #13313, #8843 ) ;
#14082 = AXIS2_PLACEMENT_3D ( 'NONE', #12240, #4275, #12165 ) ;
#14083 = CYLINDRICAL_SURFACE ( 'NONE', #304, 22.00000000000001421 ) ;
#14084 = ORIENTED_EDGE ( 'NONE', *, *, #610, .T. ) ;
#14085 = VERTEX_POINT ( 'NONE', #5866 ) ;
#14086 = AXIS2_PLACEMENT_3D ( 'NONE', #10773, #4939, #446 ) ;
#14087 = EDGE_CURVE ( 'NONE', #5893, #7269, #3216, .T. ) ;
#14088 = ORIENTED_EDGE ( 'NONE', *, *, #8742, .F. ) ;
#14089 = VECTOR ( 'NONE', #5243, 1000.000000000000000 ) ;
#14090 = EDGE_CURVE ( 'NONE', #3137, #13996, #12190, .T. ) ;
#14091 = CARTESIAN_POINT ( 'NONE',  ( 12.33230428938079903, 106.2869539367523402, 16.29453878845856707 ) ) ;
#14092 = CIRCLE ( 'NONE', #11181, 3.000000000000002665 ) ;
#14093 = DIRECTION ( 'NONE',  ( 1.000000000000000000, 0.000000000000000000, 0.000000000000000000 ) ) ;
#14094 = CIRCLE ( 'NONE', #5362, 63.00000000000000000 ) ;
#14095 = CARTESIAN_POINT ( 'NONE',  ( -37.53686968382306333, -89.89283556784496909, 10.49999999999999822 ) ) ;
#14096 = CARTESIAN_POINT ( 'NONE',  ( -70.71067811865538033, -70.71067811865414399, 8.000000000000000000 ) ) ;
#14097 = ORIENTED_EDGE ( 'NONE', *, *, #2825, .T. ) ;
#14098 = ORIENTED_EDGE ( 'NONE', *, *, #14190, .F. ) ;
#14099 = ORIENTED_EDGE ( 'NONE', *, *, #6517, .T. ) ;
#14100 = ADVANCED_FACE ( 'NONE', ( #4748 ), #13784, .F. ) ;
#14101 = LINE ( 'NONE', #3706, #1332 ) ;
#14102 = DIRECTION ( 'NONE',  ( 0.000000000000000000, 0.000000000000000000, -1.000000000000000000 ) ) ;
#14103 = AXIS2_PLACEMENT_3D ( 'NONE', #5299, #5384, #12217 ) ;
#14104 = DIRECTION ( 'NONE',  ( 0.000000000000000000, 0.000000000000000000, 1.000000000000000000 ) ) ;
#14105 = VERTEX_POINT ( 'NONE', #179 ) ;
#14106 = CIRCLE ( 'NONE', #6807, 60.50000000000000711 ) ;
#14107 = ORIENTED_EDGE ( 'NONE', *, *, #13417, .F. ) ;
#14108 = DIRECTION ( 'NONE',  ( 0.000000000000000000, 0.000000000000000000, -1.000000000000000000 ) ) ;
#14109 = ORIENTED_EDGE ( 'NONE', *, *, #5367, .F. ) ;
#14110 = ADVANCED_FACE ( 'NONE', ( #8219 ), #12637, .T. ) ;
#14111 = CARTESIAN_POINT ( 'NONE',  ( -51.19406879332065330, -13.71740939043347041, -13.00000000000000178 ) ) ;
#14112 = DIRECTION ( 'NONE',  ( 0.000000000000000000, 0.000000000000000000, 1.000000000000000000 ) ) ;
#14113 = VECTOR ( 'NONE', #1311, 1000.000000000000000 ) ;
#14114 = CARTESIAN_POINT ( 'NONE',  ( -68.58935777509427112, 68.58935777509594800, -8.000000000000000000 ) ) ;
#14115 = CARTESIAN_POINT ( 'NONE',  ( 0.000000000000000000, 0.000000000000000000, -11.74999999999999822 ) ) ;
#14116 = CARTESIAN_POINT ( 'NONE',  ( -11.45967689402250755, 74.11957758926655515, -18.06636219913714214 ) ) ;
#14117 = CARTESIAN_POINT ( 'NONE',  ( 9.706953719245472456, 57.06275842387054098, 8.000000000000000000 ) ) ;
#14118 = AXIS2_PLACEMENT_3D ( 'NONE', #14626, #3227, #13622 ) ;
#14119 = VERTEX_POINT ( 'NONE', #3830 ) ;
#14120 = CARTESIAN_POINT ( 'NONE',  ( -38.79014761921587251, 11.74264578624790190, -28.00000000000000000 ) ) ;
#14121 = ORIENTED_EDGE ( 'NONE', *, *, #7858, .T. ) ;
#14122 = ORIENTED_EDGE ( 'NONE', *, *, #3879, .F. ) ;
#14123 = AXIS2_PLACEMENT_3D ( 'NONE', #7161, #9653, #7459 ) ;
#14124 = ORIENTED_EDGE ( 'NONE', *, *, #9520, .T. ) ;
#14125 = DIRECTION ( 'NONE',  ( 0.000000000000000000, 0.000000000000000000, 1.000000000000000000 ) ) ;
#14126 = ORIENTED_EDGE ( 'NONE', *, *, #3757, .T. ) ;
#14127 = CARTESIAN_POINT ( 'NONE',  ( 89.61631465359468507, -37.12029293941410657, -13.00000000000000178 ) ) ;
#14128 = AXIS2_PLACEMENT_3D ( 'NONE', #8521, #13163, #12036 ) ;
#14129 = DIRECTION ( 'NONE',  ( 0.000000000000000000, 0.000000000000000000, -1.000000000000000000 ) ) ;
#14130 = LINE ( 'NONE', #1304, #6174 ) ;
#14131 = CYLINDRICAL_SURFACE ( 'NONE', #7028, 56.99999999999999289 ) ;
#14132 = CARTESIAN_POINT ( 'NONE',  ( 0.000000000000000000, 0.000000000000000000, -10.50000000000000000 ) ) ;
#14133 = LINE ( 'NONE', #8572, #6031 ) ;
#14134 = AXIS2_PLACEMENT_3D ( 'NONE', #9198, #8068, #13698 ) ;
#14135 = EDGE_LOOP ( 'NONE', ( #4598, #10861, #8833, #14122, #8351, #9030 ) ) ;
#14136 = EDGE_CURVE ( 'NONE', #2381, #4530, #11710, .T. ) ;
#14137 = DIRECTION ( 'NONE',  ( -0.000000000000000000, -0.000000000000000000, 1.000000000000000000 ) ) ;
#14138 = ADVANCED_FACE ( 'NONE', ( #5186 ), #14371, .F. ) ;
#14139 = VECTOR ( 'NONE', #2671, 1000.000000000000000 ) ;
#14140 = VERTEX_POINT ( 'NONE', #474 ) ;
#14141 = CARTESIAN_POINT ( 'NONE',  ( -8.156204789939931032, 106.6891793314719905, -19.96764982490488549 ) ) ;
#14142 = DIRECTION ( 'NONE',  ( -1.000000000000000000, 0.000000000000000000, 0.000000000000000000 ) ) ;
#14143 = CIRCLE ( 'NONE', #2009, 0.5000000000000004441 ) ;
#14144 = CARTESIAN_POINT ( 'NONE',  ( -20.00000000000000000, 0.000000000000000000, -28.00000000000000000 ) ) ;
#14145 = PLANE ( 'NONE',  #7606 ) ;
#14146 = AXIS2_PLACEMENT_3D ( 'NONE', #7330, #3853, #3933 ) ;
#14147 = VERTEX_POINT ( 'NONE', #11958 ) ;
#14148 = DIRECTION ( 'NONE',  ( -1.000000000000000000, 0.000000000000000000, 0.000000000000000000 ) ) ;
#14149 = ORIENTED_EDGE ( 'NONE', *, *, #11318, .T. ) ;
#14150 = CARTESIAN_POINT ( 'NONE',  ( 13.35619814848834075, -51.53979475227123430, 10.49999999999999822 ) ) ;
#14151 = DIRECTION ( 'NONE',  ( 0.000000000000000000, 0.000000000000000000, 1.000000000000000000 ) ) ;
#14152 = AXIS2_PLACEMENT_3D ( 'NONE', #4594, #5869, #3232 ) ;
#14153 = CARTESIAN_POINT ( 'NONE',  ( -25.00000000000000000, 81.24038404635962252, 16.00000000000000000 ) ) ;
#14154 = FACE_OUTER_BOUND ( 'NONE', #51, .T. ) ;
#14155 = EDGE_CURVE ( 'NONE', #14934, #14546, #7449, .T. ) ;
#14156 = ORIENTED_EDGE ( 'NONE', *, *, #8142, .T. ) ;
#14157 = DIRECTION ( 'NONE',  ( 0.000000000000000000, 0.000000000000000000, -1.000000000000000000 ) ) ;
#14158 = DIRECTION ( 'NONE',  ( 0.000000000000000000, 0.000000000000000000, -1.000000000000000000 ) ) ;
#14159 = DIRECTION ( 'NONE',  ( 1.000000000000000000, 0.000000000000000000, 0.000000000000000000 ) ) ;
#14160 = VECTOR ( 'NONE', #2522, 1000.000000000000000 ) ;
#14161 = CIRCLE ( 'NONE', #10279, 3.000000000000002665 ) ;
#14162 = ORIENTED_EDGE ( 'NONE', *, *, #4327, .T. ) ;
#14163 = ORIENTED_EDGE ( 'NONE', *, *, #10202, .F. ) ;
#14164 = DIRECTION ( 'NONE',  ( -1.000000000000000000, 0.000000000000000000, 0.000000000000000000 ) ) ;
#14165 = FACE_OUTER_BOUND ( 'NONE', #2828, .T. ) ;
#14166 = CYLINDRICAL_SURFACE ( 'NONE', #6079, 22.00000000000000355 ) ;
#14167 = DIRECTION ( 'NONE',  ( 0.000000000000000000, 0.000000000000000000, 1.000000000000000000 ) ) ;
#14168 = LINE ( 'NONE', #4992, #4995 ) ;
#14169 = AXIS2_PLACEMENT_3D ( 'NONE', #9403, #10779, #3810 ) ;
#14170 = AXIS2_PLACEMENT_3D ( 'NONE', #11815, #11739, #4901 ) ;
#14171 = CIRCLE ( 'NONE', #13215, 10.00000000000000178 ) ;
#14172 = ORIENTED_EDGE ( 'NONE', *, *, #1164, .T. ) ;
#14173 = EDGE_LOOP ( 'NONE', ( #4856, #9097, #5908, #4092 ) ) ;
#14174 = ORIENTED_EDGE ( 'NONE', *, *, #12754, .F. ) ;
#14175 = ORIENTED_EDGE ( 'NONE', *, *, #9810, .T. ) ;
#14176 = ADVANCED_FACE ( 'NONE', ( #11875 ), #10954, .F. ) ;
#14177 = CARTESIAN_POINT ( 'NONE',  ( 35.00000000000000000, 81.24038404635960831, -23.50000000000000000 ) ) ;
#14179 = ADVANCED_FACE ( 'NONE', ( #9581 ), #8378, .T. ) ;
#14178 = DIRECTION ( 'NONE',  ( 0.000000000000000000, 0.000000000000000000, 1.000000000000000000 ) ) ;
#14180 = ADVANCED_FACE ( 'NONE', ( #7379 ), #7300, .F. ) ;
#14181 = CARTESIAN_POINT ( 'NONE',  ( 69.08935777509475429, -68.58935777509547904, -13.00000000000000178 ) ) ;
#14182 = ORIENTED_EDGE ( 'NONE', *, *, #651, .F. ) ;
#14183 = CIRCLE ( 'NONE', #10055, 3.000000000000002665 ) ;
#14184 = ORIENTED_EDGE ( 'NONE', *, *, #1629, .F. ) ;
#14185 = DIRECTION ( 'NONE',  ( 0.000000000000000000, 0.000000000000000000, -1.000000000000000000 ) ) ;
#14186 = CIRCLE ( 'NONE', #9330, 44.89637028918152595 ) ;
#14187 = AXIS2_PLACEMENT_3D ( 'NONE', #12323, #14753, #6834 ) ;
#14188 = ORIENTED_EDGE ( 'NONE', *, *, #10182, .T. ) ;
#14189 = CYLINDRICAL_SURFACE ( 'NONE', #11673, 0.5000000000000004441 ) ;
#14190 = EDGE_CURVE ( 'NONE', #14620, #9479, #3947, .T. ) ;
#14191 = DIRECTION ( 'NONE',  ( 0.000000000000000000, 0.000000000000000000, 1.000000000000000000 ) ) ;
#14192 = CARTESIAN_POINT ( 'NONE',  ( 0.000000000000000000, 0.000000000000000000, -10.50000000000000000 ) ) ;
#14193 = VERTEX_POINT ( 'NONE', #9645 ) ;
#14194 = CIRCLE ( 'NONE', #7394, 63.00000000000000000 ) ;
#14195 = CARTESIAN_POINT ( 'NONE',  ( 0.000000000000000000, 0.000000000000000000, -23.50000000000000000 ) ) ;
#14196 = CARTESIAN_POINT ( 'NONE',  ( -6.123233995736766085E-15, 100.0000000000000000, 8.000000000000000000 ) ) ;
#14197 = ORIENTED_EDGE ( 'NONE', *, *, #12206, .T. ) ;
#14198 = AXIS2_PLACEMENT_3D ( 'NONE', #8453, #14301, #13095 ) ;
#14199 = DIRECTION ( 'NONE',  ( -0.000000000000000000, -0.000000000000000000, -1.000000000000000000 ) ) ;
#14200 = AXIS2_PLACEMENT_3D ( 'NONE', #6437, #689, #14587 ) ;
#14201 = EDGE_CURVE ( 'NONE', #5954, #8393, #6165, .T. ) ;
#14202 = EDGE_CURVE ( 'NONE', #14329, #2988, #13892, .T. ) ;
#14203 = VERTEX_POINT ( 'NONE', #6231 ) ;
#14204 = ORIENTED_EDGE ( 'NONE', *, *, #12718, .F. ) ;
#14205 = CIRCLE ( 'NONE', #1829, 0.5000000000000004441 ) ;
#14206 = AXIS2_PLACEMENT_3D ( 'NONE', #6809, #8106, #13659 ) ;
#14207 = DIRECTION ( 'NONE',  ( 0.000000000000000000, 0.4999999999999995559, -0.8660254037844389297 ) ) ;
#14208 = ORIENTED_EDGE ( 'NONE', *, *, #7723, .T. ) ;
#14209 = B_SPLINE_CURVE_WITH_KNOTS ( 'NONE', 3,
 ( #5546, #9867, #14818, #7738, #8952, #14513, #14744, #4111 ),
 .UNSPECIFIED., .F., .F.,
 ( 4, 2, 2, 4 ),
 ( 0.000000000000000000, 0.002450665683189817961, 0.003675998524784728459, 0.004901331366379638524 ),
 .UNSPECIFIED. ) ;
#14210 = CARTESIAN_POINT ( 'NONE',  ( 37.71449950291050612, -86.67575032682090352, 8.000000000000000000 ) ) ;
#14211 = CARTESIAN_POINT ( 'NONE',  ( 97.00000000000000000, -3.384287605079545030E-13, -8.000000000000000000 ) ) ;
#14212 = DIRECTION ( 'NONE',  ( 0.000000000000000000, -1.000000000000000000, 1.287488025362403787E-15 ) ) ;
#14213 = DIRECTION ( 'NONE',  ( -1.000000000000000000, 0.000000000000000000, 0.000000000000000000 ) ) ;
#14214 = CARTESIAN_POINT ( 'NONE',  ( -7.500000000000000888, 62.55197838597913318, 20.00000000000000000 ) ) ;
#14215 = VERTEX_POINT ( 'NONE', #556 ) ;
#14216 = AXIS2_PLACEMENT_3D ( 'NONE', #1851, #11268, #10042 ) ;
#14217 = DIRECTION ( 'NONE',  ( -0.5000000000000051070, 0.000000000000000000, 0.8660254037844355990 ) ) ;
#14218 = ORIENTED_EDGE ( 'NONE', *, *, #6193, .F. ) ;
#14219 = DIRECTION ( 'NONE',  ( 1.000000000000000000, 0.000000000000000000, 0.000000000000000000 ) ) ;
#14220 = DIRECTION ( 'NONE',  ( 0.2941176470588243164, 0.9557692240748185686, 0.000000000000000000 ) ) ;
#14221 = CARTESIAN_POINT ( 'NONE',  ( 97.00000000000000000, -3.384287605079545030E-13, -13.00000000000000178 ) ) ;
#14222 = DIRECTION ( 'NONE',  ( -1.000000000000000000, 0.000000000000000000, 0.000000000000000000 ) ) ;
#14223 = VERTEX_POINT ( 'NONE', #10872 ) ;
#14224 = VERTEX_POINT ( 'NONE', #5110 ) ;
#14225 = EDGE_CURVE ( 'NONE', #7351, #1696, #13155, .T. ) ;
#14226 = CIRCLE ( 'NONE', #8400, 2.100000000000000089 ) ;
#14227 = DIRECTION ( 'NONE',  ( -0.000000000000000000, 1.000000000000000000, -0.000000000000000000 ) ) ;
#14228 = ORIENTED_EDGE ( 'NONE', *, *, #5414, .F. ) ;
#14229 = LINE ( 'NONE', #555, #13342 ) ;
#14230 = DIRECTION ( 'NONE',  ( 1.000000000000000000, 0.000000000000000000, 0.000000000000000000 ) ) ;
#14231 = CARTESIAN_POINT ( 'NONE',  ( 0.000000000000000000, 0.000000000000000000, -10.50000000000000000 ) ) ;
#14232 = DIRECTION ( 'NONE',  ( 1.000000000000000000, 0.000000000000000000, 0.000000000000000000 ) ) ;
#14233 = ORIENTED_EDGE ( 'NONE', *, *, #9815, .T. ) ;
#14234 = VECTOR ( 'NONE', #6446, 1000.000000000000000 ) ;
#14235 = DIRECTION ( 'NONE',  ( -0.000000000000000000, -0.000000000000000000, 1.000000000000000000 ) ) ;
#14236 = DIRECTION ( 'NONE',  ( -1.000000000000000000, 0.000000000000000000, 0.000000000000000000 ) ) ;
#14237 = FACE_OUTER_BOUND ( 'NONE', #2502, .T. ) ;
#14238 = EDGE_CURVE ( 'NONE', #12729, #4183, #1280, .T. ) ;
#14239 = ORIENTED_EDGE ( 'NONE', *, *, #7960, .F. ) ;
#14240 = EDGE_CURVE ( 'NONE', #13905, #9614, #6299, .T. ) ;
#14241 = EDGE_CURVE ( 'NONE', #13345, #6195, #2482, .T. ) ;
#14242 = DIRECTION ( 'NONE',  ( -1.000000000000000000, 0.000000000000000000, 0.000000000000000000 ) ) ;
#14243 = ORIENTED_EDGE ( 'NONE', *, *, #416, .F. ) ;
#14244 = CARTESIAN_POINT ( 'NONE',  ( -24.99999999999973355, -43.30127018922208748, 8.000000000000000000 ) ) ;
#14245 = CARTESIAN_POINT ( 'NONE',  ( 8.633615064400526506, 62.40799623593409251, -19.90332611805893137 ) ) ;
#14246 = DIRECTION ( 'NONE',  ( 0.000000000000000000, 0.000000000000000000, 1.000000000000000000 ) ) ;
#14247 = CARTESIAN_POINT ( 'NONE',  ( -30.88253268887307712, 96.16299873708393875, -14.30432816676291985 ) ) ;
#14248 = EDGE_CURVE ( 'NONE', #218, #11004, #6830, .T. ) ;
#14249 = VERTEX_POINT ( 'NONE', #9506 ) ;
#14250 = VERTEX_POINT ( 'NONE', #3758 ) ;
#14251 = ORIENTED_EDGE ( 'NONE', *, *, #8062, .F. ) ;
#14252 = CYLINDRICAL_SURFACE ( 'NONE', #9563, 59.50000000000000000 ) ;
#14253 = DIRECTION ( 'NONE',  ( 1.000000000000000000, 0.000000000000000000, 0.000000000000000000 ) ) ;
#14254 = CARTESIAN_POINT ( 'NONE',  ( -41.54772703543551415, -32.26435573746212526, -10.50000000000000000 ) ) ;
#14255 = EDGE_LOOP ( 'NONE', ( #9536, #6797, #14029 ) ) ;
#14256 = ORIENTED_EDGE ( 'NONE', *, *, #9700, .F. ) ;
#14257 = DIRECTION ( 'NONE',  ( 0.000000000000000000, 0.000000000000000000, -1.000000000000000000 ) ) ;
#14258 = ORIENTED_EDGE ( 'NONE', *, *, #13256, .F. ) ;
#14259 = DIRECTION ( 'NONE',  ( 0.000000000000000000, 1.000000000000000000, -0.000000000000000000 ) ) ;
#14260 = EDGE_CURVE ( 'NONE', #2743, #6973, #6584, .T. ) ;
#14261 = DIRECTION ( 'NONE',  ( -0.000000000000000000, -0.000000000000000000, -1.000000000000000000 ) ) ;
#14262 = DIRECTION ( 'NONE',  ( -1.000000000000000000, 0.000000000000000000, 0.000000000000000000 ) ) ;
#14263 = ORIENTED_EDGE ( 'NONE', *, *, #3505, .T. ) ;
#14264 = DIRECTION ( 'NONE',  ( -0.000000000000000000, 1.000000000000000000, 0.000000000000000000 ) ) ;
#14265 = CARTESIAN_POINT ( 'NONE',  ( 37.12029293941315444, -89.61631465359504034, 8.000000000000000000 ) ) ;
#14266 = ORIENTED_EDGE ( 'NONE', *, *, #4179, .T. ) ;
#14267 = CARTESIAN_POINT ( 'NONE',  ( 99.48933418828643482, -1.674280531759671620, -8.000000000000000000 ) ) ;
#14268 = ORIENTED_EDGE ( 'NONE', *, *, #11125, .T. ) ;
#14269 = VERTEX_POINT ( 'NONE', #11260 ) ;
#14270 = CARTESIAN_POINT ( 'NONE',  ( 0.2790467552932217044, -96.58511096861892042, 10.49999999999999822 ) ) ;
#14271 = LINE ( 'NONE', #1379, #5682 ) ;
#14272 = CARTESIAN_POINT ( 'NONE',  ( 33.32140965599872118, 101.6077678005751181, -14.98557208302583099 ) ) ;
#14273 = EDGE_CURVE ( 'NONE', #9052, #8417, #8303, .T. ) ;
#14274 = EDGE_CURVE ( 'NONE', #10391, #7242, #2983, .T. ) ;
#14275 = CARTESIAN_POINT ( 'NONE',  ( -1.674280531759324342, -99.48933418828643482, -13.00000000000000178 ) ) ;
#14276 = CARTESIAN_POINT ( 'NONE',  ( 18.00000000000000355, 0.000000000000000000, -45.50000000000000000 ) ) ;
#14277 = CARTESIAN_POINT ( 'NONE',  ( 0.000000000000000000, 0.000000000000000000, 14.49999999999999822 ) ) ;
#14278 = CYLINDRICAL_SURFACE ( 'NONE', #7727, 63.00000000000000000 ) ;
#14279 = ORIENTED_EDGE ( 'NONE', *, *, #11364, .T. ) ;
#14280 = EDGE_LOOP ( 'NONE', ( #9578, #14018, #6226, #14366 ) ) ;
#14281 = EDGE_CURVE ( 'NONE', #7029, #10986, #8741, .T. ) ;
#14282 = LINE ( 'NONE', #5998, #7427 ) ;
#14283 = AXIS2_PLACEMENT_3D ( 'NONE', #11, #2223, #11580 ) ;
#14284 = FACE_OUTER_BOUND ( 'NONE', #5481, .T. ) ;
#14285 = DIRECTION ( 'NONE',  ( -0.000000000000000000, -0.000000000000000000, -1.000000000000000000 ) ) ;
#14286 = DIRECTION ( 'NONE',  ( -1.000000000000000000, 6.399202155825555340E-14, 0.000000000000000000 ) ) ;
#14287 = ORIENTED_EDGE ( 'NONE', *, *, #5827, .T. ) ;
#14288 = CARTESIAN_POINT ( 'NONE',  ( 100.0000000000000000, 1.224646799147353217E-14, 13.00000000000000178 ) ) ;
#14289 = AXIS2_PLACEMENT_3D ( 'NONE', #4229, #12196, #6550 ) ;
#14290 = ORIENTED_EDGE ( 'NONE', *, *, #14190, .T. ) ;
#14291 = EDGE_CURVE ( 'NONE', #2928, #1483, #8777, .T. ) ;
#14292 = ORIENTED_EDGE ( 'NONE', *, *, #11770, .F. ) ;
#14293 = FACE_OUTER_BOUND ( 'NONE', #11175, .T. ) ;
#14294 = CARTESIAN_POINT ( 'NONE',  ( 1.674280531759324342, 99.48933418828643482, -13.00000000000000178 ) ) ;
#14295 = AXIS2_PLACEMENT_3D ( 'NONE', #8483, #1370, #6267 ) ;
#14296 = DIRECTION ( 'NONE',  ( -1.000000000000000000, 0.000000000000000000, 0.000000000000000000 ) ) ;
#14297 = CARTESIAN_POINT ( 'NONE',  ( -7.500000000000000888, 94.70348462437907244, 20.00000000000000000 ) ) ;
#14298 = CARTESIAN_POINT ( 'NONE',  ( -7.787692492290227975, 94.68070094645281642, 19.99999999999999645 ) ) ;
#14299 = ORIENTED_EDGE ( 'NONE', *, *, #2900, .F. ) ;
#14300 = CARTESIAN_POINT ( 'NONE',  ( 19.99999999999999645, 64.99230723708768664, -26.00000000000000000 ) ) ;
#14301 = DIRECTION ( 'NONE',  ( 0.000000000000000000, 0.000000000000000000, -1.000000000000000000 ) ) ;
#14302 = VECTOR ( 'NONE', #2951, 1000.000000000000000 ) ;
#14303 = FACE_OUTER_BOUND ( 'NONE', #11479, .T. ) ;
#14304 = AXIS2_PLACEMENT_3D ( 'NONE', #4814, #4593, #9428 ) ;
#14305 = CIRCLE ( 'NONE', #248, 56.99999999999999289 ) ;
#14306 = VERTEX_POINT ( 'NONE', #1910 ) ;
#14307 = DIRECTION ( 'NONE',  ( 0.000000000000000000, 0.000000000000000000, -1.000000000000000000 ) ) ;
#14308 = EDGE_LOOP ( 'NONE', ( #11377, #9457, #2025, #1804 ) ) ;
#14309 = CYLINDRICAL_SURFACE ( 'NONE', #8842, 3.000000000000002665 ) ;
#14310 = CIRCLE ( 'NONE', #10191, 95.00000000000001421 ) ;
#14311 = CARTESIAN_POINT ( 'NONE',  ( 11.08335940112994855, 62.01770010158974600, -18.49860775790518730 ) ) ;
#14312 = DIRECTION ( 'NONE',  ( 0.000000000000000000, 0.000000000000000000, 1.000000000000000000 ) ) ;
#14313 = DIRECTION ( 'NONE',  ( -1.000000000000000000, 0.000000000000000000, 6.123233995736766036E-17 ) ) ;
#14314 = CARTESIAN_POINT ( 'NONE',  ( -31.32121808728248524, 96.02101045561126114, -14.76552927760546829 ) ) ;
#14315 = AXIS2_PLACEMENT_3D ( 'NONE', #10563, #4728, #12549 ) ;
#14316 = ORIENTED_EDGE ( 'NONE', *, *, #12268, .F. ) ;
#14317 = EDGE_CURVE ( 'NONE', #9910, #9388, #11120, .T. ) ;
#14318 = FACE_OUTER_BOUND ( 'NONE', #5006, .T. ) ;
#14320 = EDGE_CURVE ( 'NONE', #11466, #9114, #9959, .T. ) ;
#14319 = CARTESIAN_POINT ( 'NONE',  ( 0.000000000000000000, 0.000000000000000000, -10.50000000000000000 ) ) ;
#14321 = CARTESIAN_POINT ( 'NONE',  ( 52.83493649053890806, -6.470413585629217057E-15, -11.74999999999999822 ) ) ;
#14322 = ORIENTED_EDGE ( 'NONE', *, *, #3895, .F. ) ;
#14323 = CIRCLE ( 'NONE', #8047, 3.000000000000002665 ) ;
#14324 = CIRCLE ( 'NONE', #12874, 63.00000000000000000 ) ;
#14325 = ORIENTED_EDGE ( 'NONE', *, *, #14317, .F. ) ;
#14326 = DIRECTION ( 'NONE',  ( 0.000000000000000000, 0.000000000000000000, 1.000000000000000000 ) ) ;
#14327 = ADVANCED_FACE ( 'NONE', ( #867 ), #9041, .F. ) ;
#14328 = CIRCLE ( 'NONE', #7780, 100.0000000000000000 ) ;
#14329 = VERTEX_POINT ( 'NONE', #4352 ) ;
#14330 = VECTOR ( 'NONE', #14491, 1000.000000000000000 ) ;
#14331 = DIRECTION ( 'NONE',  ( 1.000000000000000000, 0.000000000000000000, 0.000000000000000000 ) ) ;
#14332 = DIRECTION ( 'NONE',  ( 1.000000000000000000, 0.000000000000000000, 0.000000000000000000 ) ) ;
#14333 = PRODUCT_DEFINITION ( 'UNKNOWN', '', #12120, #4065 ) ;
#14334 = SURFACE_SIDE_STYLE ('',( #149 ) ) ;
#14336 = CIRCLE ( 'NONE', #2700, 56.99999999999999289 ) ;
#14335 = FACE_OUTER_BOUND ( 'NONE', #4142, .T. ) ;
#14337 = DIRECTION ( 'NONE',  ( 0.000000000000000000, 0.000000000000000000, 1.000000000000000000 ) ) ;
#14338 = ORIENTED_EDGE ( 'NONE', *, *, #5009, .T. ) ;
#14339 = ADVANCED_FACE ( 'NONE', ( #8895 ), #9879, .T. ) ;
#14340 = VECTOR ( 'NONE', #2240, 1000.000000000000114 ) ;
#14341 = DIRECTION ( 'NONE',  ( -0.000000000000000000, -0.000000000000000000, -1.000000000000000000 ) ) ;
#14342 = AXIS2_PLACEMENT_3D ( 'NONE', #3600, #3451, #12854 ) ;
#14343 = VERTEX_POINT ( 'NONE', #12397 ) ;
#14344 = EDGE_LOOP ( 'NONE', ( #9146, #14555, #11780, #5529 ) ) ;
#14345 = CARTESIAN_POINT ( 'NONE',  ( 49.00442420935993226, -30.80502811811213704, -13.00000000000000178 ) ) ;
#14346 = CIRCLE ( 'NONE', #11460, 59.50000000000000711 ) ;
#14347 = CARTESIAN_POINT ( 'NONE',  ( 31.47058823529413374, 102.2673069760056848, -11.33189534135685328 ) ) ;
#14348 = CIRCLE ( 'NONE', #11465, 3.000000000000002665 ) ;
#14349 = DIRECTION ( 'NONE',  ( 0.000000000000000000, 0.000000000000000000, 1.000000000000000000 ) ) ;
#14350 = CARTESIAN_POINT ( 'NONE',  ( -45.96504489225991819, 23.50071946824089153, 8.000000000000000000 ) ) ;
#14351 = CARTESIAN_POINT ( 'NONE',  ( -99.48933418828642061, 1.674280531760365065, 8.000000000000000000 ) ) ;
#14352 = CARTESIAN_POINT ( 'NONE',  ( -6.852625091552704717, -52.05085522212505111, -10.50000000000000000 ) ) ;
#14353 = ORIENTED_EDGE ( 'NONE', *, *, #2825, .F. ) ;
#14354 = CYLINDRICAL_SURFACE ( 'NONE', #3180, 3.000000000000002665 ) ;
#14355 = ORIENTED_EDGE ( 'NONE', *, *, #1378, .T. ) ;
#14356 = DIRECTION ( 'NONE',  ( 0.000000000000000000, 0.000000000000000000, 1.000000000000000000 ) ) ;
#14357 = DIRECTION ( 'NONE',  ( -1.000000000000000000, 1.765157221169382734E-15, 0.000000000000000000 ) ) ;
#14358 = EDGE_CURVE ( 'NONE', #8214, #8032, #3457, .T. ) ;
#14359 = EDGE_CURVE ( 'NONE', #10752, #5875, #2727, .T. ) ;
#14360 = VECTOR ( 'NONE', #13088, 1000.000000000000114 ) ;
#14361 = ORIENTED_EDGE ( 'NONE', *, *, #1797, .F. ) ;
#14362 = CARTESIAN_POINT ( 'NONE',  ( 52.54657765281197612, -6.917888187662545540, -10.50000000000000000 ) ) ;
#14363 = ORIENTED_EDGE ( 'NONE', *, *, #10575, .T. ) ;
#14364 = CARTESIAN_POINT ( 'NONE',  ( -0.6666666666666660745, -4.233901974057272533, -3.300726591567089141 ) ) ;
#14365 = EDGE_CURVE ( 'NONE', #10761, #5962, #1524, .T. ) ;
#14366 = ORIENTED_EDGE ( 'NONE', *, *, #14713, .F. ) ;
#14367 = DIRECTION ( 'NONE',  ( 1.000000000000000000, 0.000000000000000000, 0.000000000000000000 ) ) ;
#14368 = EDGE_LOOP ( 'NONE', ( #8889, #2537, #14121, #8831 ) ) ;
#14369 = CIRCLE ( 'NONE', #2969, 3.000000000000002665 ) ;
#14370 = DIRECTION ( 'NONE',  ( 1.000000000000000000, 0.000000000000000000, 0.000000000000000000 ) ) ;
#14371 = CYLINDRICAL_SURFACE ( 'NONE', #9263, 10.00000000000000178 ) ;
#14372 = ADVANCED_FACE ( 'NONE', ( #6605 ), #5489, .F. ) ;
#14373 = DIRECTION ( 'NONE',  ( -1.000000000000000000, 2.682261509073382730E-15, 0.000000000000000000 ) ) ;
#14374 = DIRECTION ( 'NONE',  ( 1.000000000000000000, 0.000000000000000000, 0.000000000000000000 ) ) ;
#14375 = CYLINDRICAL_SURFACE ( 'NONE', #5853, 2.649999999999993694 ) ;
#14376 = AXIS2_PLACEMENT_3D ( 'NONE', #11981, #1347, #10750 ) ;
#14377 = EDGE_LOOP ( 'NONE', ( #7677, #11986, #716, #10360, #11850 ) ) ;
#14378 = CARTESIAN_POINT ( 'NONE',  ( 0.000000000000000000, 0.000000000000000000, 10.50000000000000000 ) ) ;
#14379 = FACE_OUTER_BOUND ( 'NONE', #731, .T. ) ;
#14380 = AXIS2_PLACEMENT_3D ( 'NONE', #9972, #14763, #8903 ) ;
#14381 = ADVANCED_FACE ( 'NONE', ( #10113 ), #13382, .T. ) ;
#14382 = CARTESIAN_POINT ( 'NONE',  ( -38.26834323650768255, 92.38795325112920409, -8.000000000000000000 ) ) ;
#14383 = CIRCLE ( 'NONE', #12203, 60.49999999999999289 ) ;
#14384 = UNCERTAINTY_MEASURE_WITH_UNIT (LENGTH_MEASURE( 1.000000000000000082E-05 ), #278, 'distance_accuracy_value', 'NONE');
#14385 = ORIENTED_EDGE ( 'NONE', *, *, #5535, .F. ) ;
#14386 = FACE_OUTER_BOUND ( 'NONE', #13897, .T. ) ;
#14387 = CIRCLE ( 'NONE', #5428, 56.99999999999999289 ) ;
#14388 = ORIENTED_EDGE ( 'NONE', *, *, #1665, .T. ) ;
#14389 = FACE_OUTER_BOUND ( 'NONE', #12672, .T. ) ;
#14390 = CARTESIAN_POINT ( 'NONE',  ( -8.075966873893682063, 74.56617093413656505, 19.99999999999999645 ) ) ;
#14391 = AXIS2_PLACEMENT_3D ( 'NONE', #10757, #2019, #5516 ) ;
#14392 = DIRECTION ( 'NONE',  ( 1.000000000000000000, 0.000000000000000000, 0.000000000000000000 ) ) ;
#14393 = CARTESIAN_POINT ( 'NONE',  ( -2.000000000000008882, 3.464101615137750390, 0.000000000000000000 ) ) ;
#14394 = DIRECTION ( 'NONE',  ( -1.000000000000000000, 0.000000000000000000, 6.123233995736766036E-17 ) ) ;
#14395 = CARTESIAN_POINT ( 'NONE',  ( 97.50000000000000000, -3.384287605079545030E-13, 10.49999999999999822 ) ) ;
#14396 = ORIENTED_EDGE ( 'NONE', *, *, #12705, .F. ) ;
#14397 = AXIS2_PLACEMENT_3D ( 'NONE', #13702, #7918, #7986 ) ;
#14398 = DIRECTION ( 'NONE',  ( -1.000000000000000000, 0.000000000000000000, 0.000000000000000000 ) ) ;
#14399 = CYLINDRICAL_SURFACE ( 'NONE', #3019, 63.00000000000000000 ) ;
#14400 = AXIS2_PLACEMENT_3D ( 'NONE', #640, #13464, #12327 ) ;
#14401 = DIRECTION ( 'NONE',  ( 0.000000000000000000, 0.000000000000000000, 1.000000000000000000 ) ) ;
#14402 = ORIENTED_EDGE ( 'NONE', *, *, #1460, .T. ) ;
#14403 = VERTEX_POINT ( 'NONE', #14829 ) ;
#14404 = FACE_OUTER_BOUND ( 'NONE', #527, .T. ) ;
#14405 = EDGE_LOOP ( 'NONE', ( #4088, #1173, #6926, #7801, #14156, #1552, #14363, #12275, #6105 ) ) ;
#14406 = EDGE_CURVE ( 'NONE', #4070, #297, #805, .T. ) ;
#14407 = AXIS2_PLACEMENT_3D ( 'NONE', #5813, #9091, #3625 ) ;
#14408 = AXIS2_PLACEMENT_3D ( 'NONE', #5661, #11528, #1408 ) ;
#14410 = CARTESIAN_POINT ( 'NONE',  ( 68.58935777509475429, -68.58935777509547904, -13.00000000000000178 ) ) ;
#14409 = AXIS2_PLACEMENT_3D ( 'NONE', #9541, #14191, #14332 ) ;
#14411 = AXIS2_PLACEMENT_3D ( 'NONE', #6945, #11603, #5801 ) ;
#14412 = LINE ( 'NONE', #10767, #6634 ) ;
#14413 = ORIENTED_EDGE ( 'NONE', *, *, #11980, .T. ) ;
#14414 = CYLINDRICAL_SURFACE ( 'NONE', #3183, 3.000000000000002665 ) ;
#14415 = FACE_OUTER_BOUND ( 'NONE', #8980, .T. ) ;
#14416 = VERTEX_POINT ( 'NONE', #6459 ) ;
#14417 = CARTESIAN_POINT ( 'NONE',  ( 56.43380494353997534, 12.86891638962136319, 8.000000000000000000 ) ) ;
#14418 = AXIS2_PLACEMENT_3D ( 'NONE', #6923, #10418, #4583 ) ;
#14419 = CIRCLE ( 'NONE', #3514, 3.000000000000002665 ) ;
#14420 = ORIENTED_EDGE ( 'NONE', *, *, #14844, .T. ) ;
#14421 = AXIS2_PLACEMENT_3D ( 'NONE', #12774, #5847, #5769 ) ;
#14422 = ORIENTED_EDGE ( 'NONE', *, *, #7072, .T. ) ;
#14423 = CARTESIAN_POINT ( 'NONE',  ( 0.000000000000000000, 0.000000000000000000, 26.00000000000000000 ) ) ;
#14424 = ORIENTED_EDGE ( 'NONE', *, *, #3665, .T. ) ;
#14425 = EDGE_CURVE ( 'NONE', #14021, #13716, #4431, .T. ) ;
#14426 = ADVANCED_FACE ( 'NONE', ( #1772 ), #6378, .T. ) ;
#14427 = CYLINDRICAL_SURFACE ( 'NONE', #4855, 3.000000000000002665 ) ;
#14428 = AXIS2_PLACEMENT_3D ( 'NONE', #3427, #1220, #2 ) ;
#14429 = CARTESIAN_POINT ( 'NONE',  ( 54.55500000000000682, 3.061616997868366378E-16, -2.500000000000000444 ) ) ;
#14430 = FACE_BOUND ( 'NONE', #4551, .T. ) ;
#14431 = DIRECTION ( 'NONE',  ( 0.000000000000000000, 0.000000000000000000, 1.000000000000000000 ) ) ;
#14432 = ADVANCED_FACE ( 'NONE', ( #11714 ), #3356, .T. ) ;
#14433 = CIRCLE ( 'NONE', #1343, 3.000000000000002665 ) ;
#14434 = CIRCLE ( 'NONE', #14421, 0.5000000000000004441 ) ;
#14435 = CARTESIAN_POINT ( 'NONE',  ( -22.33583958711380646, -30.74264578624812927, 14.49999999999999822 ) ) ;
#14436 = EDGE_LOOP ( 'NONE', ( #2678, #612, #102, #10306, #6691, #13631 ) ) ;
#14437 = CARTESIAN_POINT ( 'NONE',  ( -31.47058823529412663, 102.2673069760056421, 31.00000000000000000 ) ) ;
#14438 = CARTESIAN_POINT ( 'NONE',  ( -50.71110588017612741, -13.58799986788221226, -10.50000000000000000 ) ) ;
#14439 = DIRECTION ( 'NONE',  ( 0.000000000000000000, 0.000000000000000000, 1.000000000000000000 ) ) ;
#14440 = CYLINDRICAL_SURFACE ( 'NONE', #13176, 75.00000000000001421 ) ;
#14441 = CIRCLE ( 'NONE', #6918, 0.5000000000000004441 ) ;
#14442 = ORIENTED_EDGE ( 'NONE', *, *, #131, .T. ) ;
#14443 = DIRECTION ( 'NONE',  ( -0.000000000000000000, -0.000000000000000000, 1.000000000000000000 ) ) ;
#14444 = ORIENTED_EDGE ( 'NONE', *, *, #1529, .F. ) ;
#14445 = CARTESIAN_POINT ( 'NONE',  ( -12.50000000000000000, 40.62019202317981126, -13.50000000000000178 ) ) ;
#14446 = VERTEX_POINT ( 'NONE', #2293 ) ;
#14447 = LINE ( 'NONE', #3974, #2912 ) ;
#14448 = VERTEX_POINT ( 'NONE', #6914 ) ;
#14449 = DIRECTION ( 'NONE',  ( -1.000000000000000000, 0.000000000000000000, 0.000000000000000000 ) ) ;
#14450 = FACE_OUTER_BOUND ( 'NONE', #6599, .T. ) ;
#14451 = CARTESIAN_POINT ( 'NONE',  ( 0.000000000000000000, 0.000000000000000000, 8.000000000000000000 ) ) ;
#14452 = VECTOR ( 'NONE', #141, 1000.000000000000000 ) ;
#14453 = CARTESIAN_POINT ( 'NONE',  ( -13.71740939043329277, 51.19406879332069593, 8.000000000000000000 ) ) ;
#14454 = EDGE_CURVE ( 'NONE', #5062, #5947, #14623, .T. ) ;
#14455 = DIRECTION ( 'NONE',  ( -1.000000000000000000, 0.000000000000000000, 0.000000000000000000 ) ) ;
#14456 = DIRECTION ( 'NONE',  ( -1.000000000000000000, 0.000000000000000000, 0.000000000000000000 ) ) ;
#14457 = EDGE_CURVE ( 'NONE', #14675, #5448, #8065, .T. ) ;
#14458 = ORIENTED_EDGE ( 'NONE', *, *, #647, .T. ) ;
#14459 = CARTESIAN_POINT ( 'NONE',  ( 12.07490296461409329, 74.02221379130672574, -17.09816637537096895 ) ) ;
#14460 = CARTESIAN_POINT ( 'NONE',  ( 7.500000000000000888, 106.2673515243510991, -20.00000000000000000 ) ) ;
#14461 = DIRECTION ( 'NONE',  ( -0.000000000000000000, -0.000000000000000000, 1.000000000000000000 ) ) ;
#14462 = CIRCLE ( 'NONE', #394, 22.00000000000001421 ) ;
#14463 = ADVANCED_FACE ( 'NONE', ( #13769 ), #3588, .F. ) ;
#14464 = VERTEX_POINT ( 'NONE', #6979 ) ;
#14465 = ORIENTED_EDGE ( 'NONE', *, *, #2626, .F. ) ;
#14466 = CARTESIAN_POINT ( 'NONE',  ( -47.21331623427138879, -33.48561063518577896, -10.50000000000000000 ) ) ;
#14467 = ORIENTED_EDGE ( 'NONE', *, *, #7580, .T. ) ;
#14468 = AXIS2_PLACEMENT_3D ( 'NONE', #6421, #3027, #5453 ) ;
#14469 = LINE ( 'NONE', #7464, #12971 ) ;
#14470 = DIRECTION ( 'NONE',  ( 1.000000000000000000, 0.000000000000000000, -0.000000000000000000 ) ) ;
#14471 = EDGE_CURVE ( 'NONE', #4010, #4879, #86, .T. ) ;
#14472 = CARTESIAN_POINT ( 'NONE',  ( 2.500000000000002220, 1.178949249685208533, -2.042000000000002036 ) ) ;
#14473 = ADVANCED_FACE ( 'NONE', ( #8135 ), #5707, .T. ) ;
#14474 = CARTESIAN_POINT ( 'NONE',  ( -44.79355920668832880, -31.05588327715819474, -8.000000000000000000 ) ) ;
#14475 = CARTESIAN_POINT ( 'NONE',  ( -32.92366211674482912, 95.48362627681295578, -15.74283067514923751 ) ) ;
#14476 = CIRCLE ( 'NONE', #7916, 2.649999999999993694 ) ;
#14477 = ORIENTED_EDGE ( 'NONE', *, *, #14758, .T. ) ;
#14478 = ORIENTED_EDGE ( 'NONE', *, *, #7008, .T. ) ;
#14479 = DIRECTION ( 'NONE',  ( 0.000000000000000000, 0.000000000000000000, -1.000000000000000000 ) ) ;
#14480 = DIRECTION ( 'NONE',  ( 0.000000000000000000, 0.000000000000000000, 1.000000000000000000 ) ) ;
#14481 = DIRECTION ( 'NONE',  ( -1.000000000000000000, 0.000000000000000000, 0.000000000000000000 ) ) ;
#14482 = ORIENTED_EDGE ( 'NONE', *, *, #6481, .T. ) ;
#14483 = ADVANCED_FACE ( 'NONE', ( #12839 ), #10340, .F. ) ;
#14484 = ORIENTED_EDGE ( 'NONE', *, *, #13833, .T. ) ;
#14485 = CARTESIAN_POINT ( 'NONE',  ( 12.39897948556635399, 61.76783392443435616, -16.00000000000000000 ) ) ;
#14486 = VERTEX_POINT ( 'NONE', #2430 ) ;
#14487 = LINE ( 'NONE', #11141, #2294 ) ;
#14488 = DIRECTION ( 'NONE',  ( 1.000000000000000000, 0.000000000000000000, 0.000000000000000000 ) ) ;
#14489 =( NAMED_UNIT ( * ) PLANE_ANGLE_UNIT ( ) SI_UNIT ( $, .RADIAN. ) );
#14490 = ORIENTED_EDGE ( 'NONE', *, *, #14789, .T. ) ;
#14491 = DIRECTION ( 'NONE',  ( -0.000000000000000000, -0.000000000000000000, -1.000000000000000000 ) ) ;
#14492 = DIRECTION ( 'NONE',  ( 1.000000000000000000, 0.000000000000000000, 0.000000000000000000 ) ) ;
#14493 = ORIENTED_EDGE ( 'NONE', *, *, #11172, .F. ) ;
#14494 = LINE ( 'NONE', #7514, #5087 ) ;
#14495 = AXIS2_PLACEMENT_3D ( 'NONE', #12522, #2181, #11312 ) ;
#14496 = ORIENTED_EDGE ( 'NONE', *, *, #4975, .T. ) ;
#14497 = VERTEX_POINT ( 'NONE', #1013 ) ;
#14498 = CARTESIAN_POINT ( 'NONE',  ( -7.500000000000000888, 61.74746958378133144, -20.00000000000000000 ) ) ;
#14499 = PLANE ( 'NONE',  #6052 ) ;
#14500 = VECTOR ( 'NONE', #9313, 1000.000000000000000 ) ;
#14501 = DIRECTION ( 'NONE',  ( -0.000000000000000000, -0.000000000000000000, -1.000000000000000000 ) ) ;
#14502 = DIRECTION ( 'NONE',  ( 0.000000000000000000, 0.000000000000000000, 1.000000000000000000 ) ) ;
#14503 = DIRECTION ( 'NONE',  ( -0.000000000000000000, -0.000000000000000000, -1.000000000000000000 ) ) ;
#14504 = DIRECTION ( 'NONE',  ( -1.000000000000000000, 0.000000000000000000, 0.000000000000000000 ) ) ;
#14505 = ORIENTED_EDGE ( 'NONE', *, *, #5748, .T. ) ;
#14506 = EDGE_CURVE ( 'NONE', #2940, #219, #11961, .T. ) ;
#14507 = CARTESIAN_POINT ( 'NONE',  ( 37.71449950291050612, -86.67575032682090352, -13.00000000000000178 ) ) ;
#14508 = CARTESIAN_POINT ( 'NONE',  ( 0.000000000000000000, 0.000000000000000000, -79.80561291909842225 ) ) ;
#14509 = ADVANCED_FACE ( 'NONE', ( #3286 ), #7054, .F. ) ;
#14510 = EDGE_CURVE ( 'NONE', #4050, #13020, #9190, .T. ) ;
#14511 = EDGE_CURVE ( 'NONE', #23, #14464, #7907, .T. ) ;
#14512 = LINE ( 'NONE', #7440, #11327 ) ;
#14513 = CARTESIAN_POINT ( 'NONE',  ( -3.510273485745305511, -2.827716139362668635, -3.610536846335888672 ) ) ;
#14514 = VERTEX_POINT ( 'NONE', #5628 ) ;
#14515 = DIRECTION ( 'NONE',  ( 0.000000000000000000, 0.000000000000000000, 1.000000000000000000 ) ) ;
#14516 = ORIENTED_EDGE ( 'NONE', *, *, #14716, .T. ) ;
#14517 = CARTESIAN_POINT ( 'NONE',  ( 3.999999999999996447, 0.9868501483902626381, -0.09357334158579327932 ) ) ;
#14518 = VERTEX_POINT ( 'NONE', #164 ) ;
#14519 = DIRECTION ( 'NONE',  ( -1.000000000000000000, 0.000000000000000000, 0.000000000000000000 ) ) ;
#14520 = ORIENTED_EDGE ( 'NONE', *, *, #3292, .F. ) ;
#14521 = FACE_OUTER_BOUND ( 'NONE', #11123, .T. ) ;
#14522 = CYLINDRICAL_SURFACE ( 'NONE', #2666, 2.100000000000000089 ) ;
#14523 = DIRECTION ( 'NONE',  ( 0.000000000000000000, 0.000000000000000000, 1.000000000000000000 ) ) ;
#14524 = FACE_OUTER_BOUND ( 'NONE', #5917, .T. ) ;
#14525 = LINE ( 'NONE', #3980, #3978 ) ;
#14526 = ADVANCED_FACE ( 'NONE', ( #6752 ), #13992, .T. ) ;
#14527 = AXIS2_PLACEMENT_3D ( 'NONE', #13440, #13365, #7891 ) ;
#14528 = CARTESIAN_POINT ( 'NONE',  ( -12.26039456458906152, 94.20559340471635323, 16.55589812076405565 ) ) ;
#14529 = ORIENTED_EDGE ( 'NONE', *, *, #1246, .F. ) ;
#14530 = EDGE_CURVE ( 'NONE', #7147, #4198, #11578, .T. ) ;
#14531 = DIRECTION ( 'NONE',  ( 1.000000000000000000, 0.000000000000000000, 0.000000000000000000 ) ) ;
#14532 = FACE_OUTER_BOUND ( 'NONE', #11509, .T. ) ;
#14533 = CARTESIAN_POINT ( 'NONE',  ( 89.61631465359491244, 37.12029293941346708, -13.00000000000000178 ) ) ;
#14534 = ORIENTED_EDGE ( 'NONE', *, *, #12506, .F. ) ;
#14535 = CARTESIAN_POINT ( 'NONE',  ( -4.140404888673274719, -2.228338276487456859, -3.686887068327036943 ) ) ;
#14536 = AXIS2_PLACEMENT_3D ( 'NONE', #2432, #11715, #8136 ) ;
#14537 = VERTEX_POINT ( 'NONE', #4650 ) ;
#14538 = DIRECTION ( 'NONE',  ( 0.000000000000000000, 0.000000000000000000, 1.000000000000000000 ) ) ;
#14539 = DIRECTION ( 'NONE',  ( -0.5000000000000016653, 0.8660254037844378194, 0.000000000000000000 ) ) ;
#14540 = ORIENTED_EDGE ( 'NONE', *, *, #9016, .T. ) ;
#14541 = CARTESIAN_POINT ( 'NONE',  ( -52.54657765281192638, 6.917888187662934563, 10.49999999999999822 ) ) ;
#14542 = DIRECTION ( 'NONE',  ( -0.000000000000000000, -0.000000000000000000, -1.000000000000000000 ) ) ;
#14543 = DIRECTION ( 'NONE',  ( 1.000000000000000000, 0.000000000000000000, 0.000000000000000000 ) ) ;
#14544 = ORIENTED_EDGE ( 'NONE', *, *, #3385, .F. ) ;
#14545 =( GEOMETRIC_REPRESENTATION_CONTEXT ( 3 ) GLOBAL_UNCERTAINTY_ASSIGNED_CONTEXT ( ( #14384 ) ) GLOBAL_UNIT_ASSIGNED_CONTEXT ( ( #278, #4915, #11898 ) ) REPRESENTATION_CONTEXT ( 'NONE', 'WORKASPACE' ) );
#14546 = VERTEX_POINT ( 'NONE', #5771 ) ;
#14547 = CIRCLE ( 'NONE', #983, 0.5000000000000004441 ) ;
#14548 = ORIENTED_EDGE ( 'NONE', *, *, #1951, .T. ) ;
#14549 =( REPRESENTATION_RELATIONSHIP ('NONE','NONE', #12187, #12767 ) REPRESENTATION_RELATIONSHIP_WITH_TRANSFORMATION ( #6707 )SHAPE_REPRESENTATION_RELATIONSHIP( ) );
#14550 = FACE_OUTER_BOUND ( 'NONE', #7068, .T. ) ;
#14551 = CIRCLE ( 'NONE', #4605, 0.5000000000000004441 ) ;
#14552 = CARTESIAN_POINT ( 'NONE',  ( 0.000000000000000000, 0.000000000000000000, 8.000000000000000000 ) ) ;
#14553 = AXIS2_PLACEMENT_3D ( 'NONE', #4336, #7583, #690 ) ;
#14554 = FACE_OUTER_BOUND ( 'NONE', #2872, .T. ) ;
#14555 = ORIENTED_EDGE ( 'NONE', *, *, #5816, .T. ) ;
#14556 = EDGE_CURVE ( 'NONE', #14416, #8471, #13922, .T. ) ;
#14557 = ADVANCED_FACE ( 'NONE', ( #7207 ), #391, .F. ) ;
#14558 = ORIENTED_EDGE ( 'NONE', *, *, #12502, .T. ) ;
#14559 = ORIENTED_EDGE ( 'NONE', *, *, #12893, .T. ) ;
#14560 = ORIENTED_EDGE ( 'NONE', *, *, #5819, .T. ) ;
#14561 = AXIS2_PLACEMENT_3D ( 'NONE', #9932, #10012, #7805 ) ;
#14562 = ADVANCED_FACE ( 'NONE', ( #4950 ), #1674, .F. ) ;
#14563 = CIRCLE ( 'NONE', #745, 59.50000000000000000 ) ;
#14564 = DIRECTION ( 'NONE',  ( 0.000000000000000000, 0.000000000000000000, -1.000000000000000000 ) ) ;
#14565 = AXIS2_PLACEMENT_3D ( 'NONE', #12324, #4286, #5555 ) ;
#14566 = CONICAL_SURFACE ( 'NONE', #3903, 52.83493649053890806, 0.5235987755983000369 ) ;
#14567 = DIRECTION ( 'NONE',  ( 0.000000000000000000, 0.000000000000000000, -1.000000000000000000 ) ) ;
#14568 = LINE ( 'NONE', #13422, #9849 ) ;
#14569 = EDGE_CURVE ( 'NONE', #8389, #13406, #2422, .T. ) ;
#14570 = EDGE_LOOP ( 'NONE', ( #7209, #6293 ) ) ;
#14571 = DIRECTION ( 'NONE',  ( 1.000000000000000000, 0.000000000000000000, 0.000000000000000000 ) ) ;
#14572 = CARTESIAN_POINT ( 'NONE',  ( -55.00000000000000000, 0.000000000000000000, -13.00000000000000178 ) ) ;
#14573 = ORIENTED_EDGE ( 'NONE', *, *, #1477, .F. ) ;
#14574 = AXIS2_PLACEMENT_3D ( 'NONE', #13073, #2821, #5093 ) ;
#14575 = DIRECTION ( 'NONE',  ( 0.000000000000000000, 0.000000000000000000, 1.000000000000000000 ) ) ;
#14576 = AXIS2_PLACEMENT_3D ( 'NONE', #12305, #687, #4100 ) ;
#14577 = ORIENTED_EDGE ( 'NONE', *, *, #7217, .T. ) ;
#14578 = AXIS2_PLACEMENT_3D ( 'NONE', #5706, #4794, #7974 ) ;
#14579 = EDGE_CURVE ( 'NONE', #1620, #5520, #6531, .T. ) ;
#14580 = AXIS2_PLACEMENT_3D ( 'NONE', #11972, #11053, #2919 ) ;
#14581 = EDGE_LOOP ( 'NONE', ( #1, #7953 ) ) ;
#14582 = CARTESIAN_POINT ( 'NONE',  ( 68.09867107462983427, 68.49330278050145182, -13.00000000000000178 ) ) ;
#14583 = FACE_OUTER_BOUND ( 'NONE', #5673, .T. ) ;
#14584 = CIRCLE ( 'NONE', #10689, 3.000000000000002665 ) ;
#14585 = VECTOR ( 'NONE', #7943, 1000.000000000000000 ) ;
#14586 = PRODUCT_DEFINITION_CONTEXT ( 'detailed design', #11945, 'design' ) ;
#14587 = DIRECTION ( 'NONE',  ( 1.000000000000000000, 0.000000000000000000, 0.000000000000000000 ) ) ;
#14588 = CYLINDRICAL_SURFACE ( 'NONE', #14063, 0.5000000000000022204 ) ;
#14589 = AXIS2_PLACEMENT_3D ( 'NONE', #13362, #7582, #14786 ) ;
#14590 = DIRECTION ( 'NONE',  ( -1.000000000000000000, 0.000000000000000000, 0.000000000000000000 ) ) ;
#14591 = CIRCLE ( 'NONE', #2952, 50.00000000000000000 ) ;
#14592 = ORIENTED_EDGE ( 'NONE', *, *, #5067, .F. ) ;
#14593 = FACE_BOUND ( 'NONE', #2191, .T. ) ;
#14594 = PRODUCT_DEFINITION_SHAPE ( 'NONE', 'NONE',  #15038 ) ;
#14595 = ORIENTED_EDGE ( 'NONE', *, *, #8001, .F. ) ;
#14596 = CARTESIAN_POINT ( 'NONE',  ( 36.14014761921570340, 11.74264578624841171, -25.50000000000000355 ) ) ;
#14597 = CARTESIAN_POINT ( 'NONE',  ( -6.526309611002575117, -49.57224306869051844, -8.000000000000000000 ) ) ;
#14598 = ORIENTED_EDGE ( 'NONE', *, *, #12649, .T. ) ;
#14599 = CARTESIAN_POINT ( 'NONE',  ( 42.64958156413651835, 32.39328945492032830, -10.50000000000000000 ) ) ;
#14600 = FACE_OUTER_BOUND ( 'NONE', #2602, .T. ) ;
#14601 = CIRCLE ( 'NONE', #6333, 59.50000000000000711 ) ;
#14602 = EDGE_LOOP ( 'NONE', ( #281, #1271, #9625, #4026 ) ) ;
#14603 = PLANE ( 'NONE',  #9936 ) ;
#14604 = EDGE_CURVE ( 'NONE', #8687, #8824, #2905, .T. ) ;
#14605 = EDGE_LOOP ( 'NONE', ( #3350, #14854, #12675, #9228 ) ) ;
#14606 = DIRECTION ( 'NONE',  ( 0.000000000000000000, 0.000000000000000000, 1.000000000000000000 ) ) ;
#14607 = DIRECTION ( 'NONE',  ( 1.000000000000000000, 0.000000000000000000, -0.000000000000000000 ) ) ;
#14608 = EDGE_CURVE ( 'NONE', #11469, #13059, #14804, .T. ) ;
#14609 = CARTESIAN_POINT ( 'NONE',  ( -12.86891638962156215, 56.43380494353993271, 10.49999999999999822 ) ) ;
#14610 = EDGE_CURVE ( 'NONE', #6323, #14678, #9439, .T. ) ;
#14611 = AXIS2_PLACEMENT_3D ( 'NONE', #10021, #3121, #3052 ) ;
#14612 = CARTESIAN_POINT ( 'NONE',  ( 57.06275842387049835, -9.706953719245678514, -10.50000000000000000 ) ) ;
#14613 = CARTESIAN_POINT ( 'NONE',  ( -29.26435573746199381, 42.04772703543562073, -8.000000000000000000 ) ) ;
#14614 = CARTESIAN_POINT ( 'NONE',  ( 25.00000000000000000, 81.24038404635960831, -23.50000000000000000 ) ) ;
#14615 = VERTEX_POINT ( 'NONE', #14351 ) ;
#14616 = AXIS2_PLACEMENT_3D ( 'NONE', #6527, #14686, #5556 ) ;
#14617 = CARTESIAN_POINT ( 'NONE',  ( 27.94117647058824616, 90.79807628710781842, -16.00000000000000000 ) ) ;
#14618 = CARTESIAN_POINT ( 'NONE',  ( 0.000000000000000000, 0.000000000000000000, 8.000000000000000000 ) ) ;
#14619 = AXIS2_PLACEMENT_3D ( 'NONE', #2844, #10879, #9435 ) ;
#14620 = VERTEX_POINT ( 'NONE', #13224 ) ;
#14621 = CARTESIAN_POINT ( 'NONE',  ( 0.02511973781850741771, -4.877415612947427981, -3.751298745799846568 ) ) ;
#14622 = ORIENTED_EDGE ( 'NONE', *, *, #2965, .T. ) ;
#14623 = CIRCLE ( 'NONE', #63, 63.00000000000000000 ) ;
#14624 = DIRECTION ( 'NONE',  ( 1.000000000000000000, 0.000000000000000000, 0.000000000000000000 ) ) ;
#14625 = EDGE_CURVE ( 'NONE', #13141, #8687, #3400, .T. ) ;
#14626 = CARTESIAN_POINT ( 'NONE',  ( 0.000000000000000000, 0.000000000000000000, -8.000000000000000000 ) ) ;
#14627 = EDGE_CURVE ( 'NONE', #14878, #8252, #3648, .T. ) ;
#14628 = CARTESIAN_POINT ( 'NONE',  ( -100.0000000000000000, 1.090307039623097308E-12, -8.000000000000000000 ) ) ;
#14629 = DIRECTION ( 'NONE',  ( 1.000000000000000000, 0.000000000000000000, 0.000000000000000000 ) ) ;
#14630 = CARTESIAN_POINT ( 'NONE',  ( 22.33583958711425055, -30.74264578624780597, -33.00000000000000000 ) ) ;
#14631 = ORIENTED_EDGE ( 'NONE', *, *, #3230, .F. ) ;
#14632 = ORIENTED_EDGE ( 'NONE', *, *, #9078, .T. ) ;
#14633 = AXIS2_PLACEMENT_3D ( 'NONE', #3076, #13539, #10044 ) ;
#14634 = CARTESIAN_POINT ( 'NONE',  ( -37.53686968382306333, -89.89283556784496909, -10.50000000000000000 ) ) ;
#14635 = DIRECTION ( 'NONE',  ( 1.000000000000000000, 0.000000000000000000, 0.000000000000000000 ) ) ;
#14636 = CYLINDRICAL_SURFACE ( 'NONE', #11736, 57.00000000000000000 ) ;
#14637 = VERTEX_POINT ( 'NONE', #14058 ) ;
#14638 = VECTOR ( 'NONE', #749, 1000.000000000000000 ) ;
#14639 = ORIENTED_EDGE ( 'NONE', *, *, #8696, .F. ) ;
#14640 = ORIENTED_EDGE ( 'NONE', *, *, #2642, .F. ) ;
#14641 = CIRCLE ( 'NONE', #12931, 2.649999999999985700 ) ;
#14642 = LINE ( 'NONE', #3097, #7120 ) ;
#14643 = CARTESIAN_POINT ( 'NONE',  ( -12.50000000000000000, 59.24038404635959409, -20.00000000000000000 ) ) ;
#14644 =( LENGTH_UNIT ( ) NAMED_UNIT ( * ) SI_UNIT ( .MILLI., .METRE. ) );
#14645 = DIRECTION ( 'NONE',  ( 1.000000000000000000, 0.000000000000000000, 0.000000000000000000 ) ) ;
#14646 = CARTESIAN_POINT ( 'NONE',  ( 0.000000000000000000, 0.000000000000000000, -8.000000000000000000 ) ) ;
#14647 = CARTESIAN_POINT ( 'NONE',  ( -26.49999999999971578, -45.89934640057541060, 10.49999999999999822 ) ) ;
#14648 = EDGE_CURVE ( 'NONE', #13160, #13122, #11400, .T. ) ;
#14649 = VERTEX_POINT ( 'NONE', #9485 ) ;
#14650 = PLANE ( 'NONE',  #12605 ) ;
#14651 = EDGE_LOOP ( 'NONE', ( #11901, #10517, #11060, #7901, #2157 ) ) ;
#14652 = EDGE_CURVE ( 'NONE', #5322, #2326, #3128, .T. ) ;
#14653 = EDGE_LOOP ( 'NONE', ( #8105, #4282, #523, #8354 ) ) ;
#14654 = ORIENTED_EDGE ( 'NONE', *, *, #10182, .F. ) ;
#14655 = CARTESIAN_POINT ( 'NONE',  ( 22.05882352941176094, 71.68269180561141241, -23.50000000000000000 ) ) ;
#14656 = VECTOR ( 'NONE', #547, 1000.000000000000000 ) ;
#14657 = CIRCLE ( 'NONE', #1557, 75.00000000000001421 ) ;
#14658 = ADVANCED_FACE ( 'NONE', ( #6067 ), #2660, .T. ) ;
#14659 = AXIS2_PLACEMENT_3D ( 'NONE', #8744, #12399, #9881 ) ;
#14660 = CARTESIAN_POINT ( 'NONE',  ( 5.204748896376250896E-15, 85.00000000000000000, 46.00000000000000000 ) ) ;
#14661 = PLANE ( 'NONE',  #8370 ) ;
#14662 = CARTESIAN_POINT ( 'NONE',  ( 37.71449950291050612, -86.67575032682090352, -8.000000000000000000 ) ) ;
#14663 = EDGE_CURVE ( 'NONE', #4331, #7416, #737, .T. ) ;
#14664 = DIRECTION ( 'NONE',  ( 1.000000000000000000, 0.000000000000000000, 0.000000000000000000 ) ) ;
#14665 = ADVANCED_FACE ( 'NONE', ( #1386 ), #13146, .F. ) ;
#14666 = ORIENTED_EDGE ( 'NONE', *, *, #7637, .T. ) ;
#14667 = AXIS2_PLACEMENT_3D ( 'NONE', #3009, #11908, #1500 ) ;
#14668 = AXIS2_PLACEMENT_3D ( 'NONE', #12669, #12587, #8101 ) ;
#14669 = DIRECTION ( 'NONE',  ( -0.000000000000000000, 0.000000000000000000, -1.000000000000000000 ) ) ;
#14670 = AXIS2_PLACEMENT_3D ( 'NONE', #968, #12512, #10519 ) ;
#14671 = CARTESIAN_POINT ( 'NONE',  ( 3.000000000000004885, -97.00000000000000000, -13.00000000000000178 ) ) ;
#14672 = FACE_OUTER_BOUND ( 'NONE', #856, .T. ) ;
#14673 = ORIENTED_EDGE ( 'NONE', *, *, #7753, .F. ) ;
#14674 =( NAMED_UNIT ( * ) SI_UNIT ( $, .STERADIAN. ) SOLID_ANGLE_UNIT ( ) );
#14675 = VERTEX_POINT ( 'NONE', #9409 ) ;
#14676 = AXIS2_PLACEMENT_3D ( 'NONE', #436, #5064, #4364 ) ;
#14677 = DIRECTION ( 'NONE',  ( -1.000000000000000000, 0.000000000000000000, 0.000000000000000000 ) ) ;
#14678 = VERTEX_POINT ( 'NONE', #10629 ) ;
#14679 = CIRCLE ( 'NONE', #10548, 3.000000000000002665 ) ;
#14680 = CARTESIAN_POINT ( 'NONE',  ( -12.07377633196514566, 61.83297368684232964, 17.10072941380094846 ) ) ;
#14681 = AXIS2_PLACEMENT_3D ( 'NONE', #7518, #12172, #14022 ) ;
#14682 = EDGE_LOOP ( 'NONE', ( #12483, #10803, #3399, #10977, #8814, #472 ) ) ;
#14683 = ORIENTED_EDGE ( 'NONE', *, *, #3943, .T. ) ;
#14684 = DIRECTION ( 'NONE',  ( -0.000000000000000000, -0.000000000000000000, -1.000000000000000000 ) ) ;
#14685 = CYLINDRICAL_SURFACE ( 'NONE', #10668, 60.50000000000000000 ) ;
#14686 = DIRECTION ( 'NONE',  ( 0.000000000000000000, 0.000000000000000000, 1.000000000000000000 ) ) ;
#14687 = DIRECTION ( 'NONE',  ( 1.000000000000000000, 0.000000000000000000, 0.000000000000000000 ) ) ;
#14688 = CARTESIAN_POINT ( 'NONE',  ( 2.500000000000002220, 1.178949249685215417, 2.042000000000002036 ) ) ;
#14689 = DIRECTION ( 'NONE',  ( 0.000000000000000000, 0.000000000000000000, 1.000000000000000000 ) ) ;
#14690 = CIRCLE ( 'NONE', #13466, 0.5000000000000004441 ) ;
#14691 = VERTEX_POINT ( 'NONE', #230 ) ;
#14692 = LINE ( 'NONE', #7527, #9591 ) ;
#14693 = CYLINDRICAL_SURFACE ( 'NONE', #838, 0.5000000000000004441 ) ;
#14694 = CIRCLE ( 'NONE', #11299, 56.99999999999998579 ) ;
#14695 = DIRECTION ( 'NONE',  ( 0.000000000000000000, 0.000000000000000000, 1.000000000000000000 ) ) ;
#14696 = ORIENTED_EDGE ( 'NONE', *, *, #2945, .F. ) ;
#14697 = VECTOR ( 'NONE', #2259, 1000.000000000000000 ) ;
#14698 = CARTESIAN_POINT ( 'NONE',  ( 26.49999999999971578, 45.89934640057541060, -10.50000000000000000 ) ) ;
#14699 = AXIS2_PLACEMENT_3D ( 'NONE', #2955, #12077, #5305 ) ;
#14700 = EDGE_LOOP ( 'NONE', ( #1242, #4681, #4199, #7572, #8244, #7644 ) ) ;
#14701 = CARTESIAN_POINT ( 'NONE',  ( 0.000000000000000000, 0.000000000000000000, -25.03750572909317285 ) ) ;
#14702 = CARTESIAN_POINT ( 'NONE',  ( -20.00000000000000000, 0.000000000000000000, 13.00000000000000178 ) ) ;
#14703 = B_SPLINE_CURVE_WITH_KNOTS ( 'NONE', 3,
 ( #7483, #10840, #372, #4016, #7188, #13276 ),
 .UNSPECIFIED., .F., .F.,
 ( 4, 2, 4 ),
 ( -3.640115492410510249E-06, 0.0002066546034003379048, 0.0004169493222930863250 ),
 .UNSPECIFIED. ) ;
#14704 = DIRECTION ( 'NONE',  ( 1.000000000000000000, 0.000000000000000000, 0.000000000000000000 ) ) ;
#14705 = DIRECTION ( 'NONE',  ( 1.000000000000000000, 0.000000000000000000, 0.000000000000000000 ) ) ;
#14706 = APPLICATION_PROTOCOL_DEFINITION ( 'draft international standard', 'automotive_design', 1998, #9976 ) ;
#14707 = ORIENTED_EDGE ( 'NONE', *, *, #5739, .T. ) ;
#14708 = ORIENTED_EDGE ( 'NONE', *, *, #3721, .F. ) ;
#14709 = ORIENTED_EDGE ( 'NONE', *, *, #3799, .F. ) ;
#14710 = AXIS2_PLACEMENT_3D ( 'NONE', #13719, #7932, #15006 ) ;
#14711 = DIRECTION ( 'NONE',  ( 1.000000000000000000, 0.000000000000000000, 0.000000000000000000 ) ) ;
#14712 = FACE_OUTER_BOUND ( 'NONE', #4606, .T. ) ;
#14713 = EDGE_CURVE ( 'NONE', #8537, #14933, #3738, .T. ) ;
#14714 = DIRECTION ( 'NONE',  ( 0.000000000000000000, 0.000000000000000000, 1.000000000000000000 ) ) ;
#14715 = EDGE_CURVE ( 'NONE', #5499, #10220, #6668, .T. ) ;
#14717 = EDGE_LOOP ( 'NONE', ( #14338, #9275, #2158, #14573 ) ) ;
#14716 = EDGE_CURVE ( 'NONE', #9289, #8417, #5246, .T. ) ;
#14718 = VERTEX_POINT ( 'NONE', #7730 ) ;
#14719 = ORIENTED_EDGE ( 'NONE', *, *, #2626, .T. ) ;
#14720 = AXIS2_PLACEMENT_3D ( 'NONE', #2300, #13773, #5638 ) ;
#14721 = EDGE_CURVE ( 'NONE', #1683, #4112, #4846, .T. ) ;
#14722 = DIRECTION ( 'NONE',  ( -1.000000000000000000, 6.308085367188389255E-16, 0.000000000000000000 ) ) ;
#14723 = CARTESIAN_POINT ( 'NONE',  ( 91.27544013909738396, -39.61975340586589311, -8.000000000000000000 ) ) ;
#14724 =( BOUNDED_SURFACE ( )  B_SPLINE_SURFACE ( 3, 2, ( 
 ( #2295, #87, #9344 ),
 ( #8206, #13923, #8281 ),
 ( #5850, #12921, #2513 ),
 ( #13770, #3517, #7134 ),
 ( #3357, #7976, #6837 ),
 ( #11496, #1096, #10342 ) ),
 .UNSPECIFIED., .F., .F., .F. ) 
 B_SPLINE_SURFACE_WITH_KNOTS ( ( 4, 2, 4 ),
 ( 3, 3 ),
 ( 0.02027752710269158445, 0.02273781595091097299, 0.02519810479913036153 ),
 ( 0.000000000000000000, 1.000000000000000000 ),
 .UNSPECIFIED. ) 
 GEOMETRIC_REPRESENTATION_ITEM ( )  RATIONAL_B_SPLINE_SURFACE ( (
 ( 1.000000000000000000, 0.8047781431712808242, 1.000000000000000000),
 ( 1.000000000000000000, 0.8123773247082141102, 1.000000000000000000),
 ( 1.000000000000000000, 0.8190670192157281093, 1.000000000000000000),
 ( 1.000000000000000000, 0.8192353552909803494, 1.000000000000000000),
 ( 1.000000000000000000, 0.8126132098228610046, 1.000000000000000000),
 ( 1.000000000000000000, 0.8047712465856391439, 1.000000000000000000) ) ) 
 REPRESENTATION_ITEM ( '' )  SURFACE ( )  );
#14725 = FILL_AREA_STYLE ('',( #11225 ) ) ;
#14726 = CARTESIAN_POINT ( 'NONE',  ( 49.00442420935993226, -30.80502811811213704, -10.50000000000000000 ) ) ;
#14727 = VERTEX_POINT ( 'NONE', #2882 ) ;
#14728 = CARTESIAN_POINT ( 'NONE',  ( 0.000000000000000000, 2.357898499370430834, 0.000000000000000000 ) ) ;
#14729 = CARTESIAN_POINT ( 'NONE',  ( -34.64620656398767551, 101.0151817716822507, 15.74933755401541902 ) ) ;
#14730 = VERTEX_POINT ( 'NONE', #1824 ) ;
#14731 = CARTESIAN_POINT ( 'NONE',  ( 2.345747346278116208, -3.264484291692499429, -0.01223254789874357248 ) ) ;
#14732 = EDGE_LOOP ( 'NONE', ( #10031, #14420, #10717, #13281, #4378 ) ) ;
#14733 = EDGE_LOOP ( 'NONE', ( #6428, #13129, #13170, #14769, #4564, #3474, #7709, #12560, #1281, #1375 ) ) ;
#14734 = FACE_OUTER_BOUND ( 'NONE', #10945, .T. ) ;
#14735 = EDGE_CURVE ( 'NONE', #9586, #14514, #11322, .T. ) ;
#14736 = DIRECTION ( 'NONE',  ( 0.000000000000000000, 0.000000000000000000, -1.000000000000000000 ) ) ;
#14737 = UNCERTAINTY_MEASURE_WITH_UNIT (LENGTH_MEASURE( 1.000000000000000082E-05 ), #3058, 'distance_accuracy_value', 'NONE');
#14738 = CARTESIAN_POINT ( 'NONE',  ( 54.55500000000000682, 0.000000000000000000, 0.000000000000000000 ) ) ;
#14739 = CARTESIAN_POINT ( 'NONE',  ( -71.53347797788819662, -69.16568774265570596, -13.00000000000000178 ) ) ;
#14740 = CARTESIAN_POINT ( 'NONE',  ( 25.00000000000000000, 81.24038404635960831, -26.00000000000000000 ) ) ;
#14741 = ORIENTED_EDGE ( 'NONE', *, *, #13189, .F. ) ;
#14742 = FACE_OUTER_BOUND ( 'NONE', #3105, .T. ) ;
#14743 = DIRECTION ( 'NONE',  ( -1.000000000000000000, 0.000000000000000000, 0.000000000000000000 ) ) ;
#14744 = CARTESIAN_POINT ( 'NONE',  ( -3.861362476283254352, -2.629030857716006420, -3.671615880910374052 ) ) ;
#14745 = ORIENTED_EDGE ( 'NONE', *, *, #7488, .T. ) ;
#14746 = CARTESIAN_POINT ( 'NONE',  ( 0.000000000000000000, 0.000000000000000000, -10.50000000000000000 ) ) ;
#14747 = ORIENTED_EDGE ( 'NONE', *, *, #11866, .F. ) ;
#14748 = EDGE_CURVE ( 'NONE', #5824, #9024, #2178, .T. ) ;
#14749 = DIRECTION ( 'NONE',  ( 0.000000000000000000, 0.000000000000000000, -1.000000000000000000 ) ) ;
#14750 = ADVANCED_FACE ( 'NONE', ( #4266 ), #1750, .T. ) ;
#14751 = ORIENTED_EDGE ( 'NONE', *, *, #1309, .T. ) ;
#14752 = CARTESIAN_POINT ( 'NONE',  ( 1.674280531759317014, -94.51066581171355097, -8.000000000000000000 ) ) ;
#14753 = DIRECTION ( 'NONE',  ( 0.000000000000000000, 0.000000000000000000, 1.000000000000000000 ) ) ;
#14754 = CARTESIAN_POINT ( 'NONE',  ( -0.6937372685066672817, 4.453844082567719909, -3.610536846335887340 ) ) ;
#14755 = CARTESIAN_POINT ( 'NONE',  ( -57.06275842387042729, 9.706953719246069312, -13.00000000000000178 ) ) ;
#14756 = DIRECTION ( 'NONE',  ( 0.000000000000000000, 0.000000000000000000, 1.000000000000000000 ) ) ;
#14757 = CARTESIAN_POINT ( 'NONE',  ( 9.706953719245472456, 57.06275842387054098, -10.50000000000000000 ) ) ;
#14758 = EDGE_CURVE ( 'NONE', #13178, #9373, #4127, .T. ) ;
#14759 = CARTESIAN_POINT ( 'NONE',  ( -13.71740939043329277, 51.19406879332069593, 10.49999999999999822 ) ) ;
#14760 = ORIENTED_EDGE ( 'NONE', *, *, #1396, .T. ) ;
#14761 = LINE ( 'NONE', #10348, #2591 ) ;
#14762 = CARTESIAN_POINT ( 'NONE',  ( 10.44268084954786069, 94.42456965614839248, -19.05230465901501091 ) ) ;
#14763 = DIRECTION ( 'NONE',  ( 0.000000000000000000, 0.000000000000000000, -1.000000000000000000 ) ) ;
#14764 = AXIS2_PLACEMENT_3D ( 'NONE', #14895, #1218, #8046 ) ;
#14765 = DIRECTION ( 'NONE',  ( 0.000000000000000000, 0.000000000000000000, 1.000000000000000000 ) ) ;
#14766 = ADVANCED_FACE ( 'NONE', ( #12156 ), #14588, .F. ) ;
#14767 = ORIENTED_EDGE ( 'NONE', *, *, #12830, .T. ) ;
#14768 = DIRECTION ( 'NONE',  ( 0.000000000000000000, 1.000000000000000000, 0.000000000000000000 ) ) ;
#14769 = ORIENTED_EDGE ( 'NONE', *, *, #6467, .T. ) ;
#14770 = CARTESIAN_POINT ( 'NONE',  ( -68.68541276968778675, 69.08004447556137961, 10.49999999999999822 ) ) ;
#14771 = DIRECTION ( 'NONE',  ( 0.000000000000000000, 0.000000000000000000, -1.000000000000000000 ) ) ;
#14772 = CARTESIAN_POINT ( 'NONE',  ( 8.154413083459850498, 106.6893057894985617, -19.96764870088429689 ) ) ;
#14773 = CARTESIAN_POINT ( 'NONE',  ( 0.000000000000000000, 0.000000000000000000, -10.50000000000000000 ) ) ;
#14774 = ITEM_DEFINED_TRANSFORMATION ( 'NONE', 'NONE', #7734,  #5108 ) ;
#14775 = ORIENTED_EDGE ( 'NONE', *, *, #5632, .F. ) ;
#14776 = ORIENTED_EDGE ( 'NONE', *, *, #3505, .F. ) ;
#14777 = CYLINDRICAL_SURFACE ( 'NONE', #9832, 5.000000000000000888 ) ;
#14778 = DIRECTION ( 'NONE',  ( -1.000000000000000000, 0.000000000000000000, 0.000000000000000000 ) ) ;
#14779 = CARTESIAN_POINT ( 'NONE',  ( 27.94117647058824616, 90.79807628710781842, -23.50000000000000000 ) ) ;
#14780 = VERTEX_POINT ( 'NONE', #8717 ) ;
#14781 = AXIS2_PLACEMENT_3D ( 'NONE', #9411, #13843, #14910 ) ;
#14782 = ORIENTED_EDGE ( 'NONE', *, *, #2830, .T. ) ;
#14783 = EDGE_LOOP ( 'NONE', ( #10969, #3313, #13972, #3377, #8605 ) ) ;
#14784 = FACE_OUTER_BOUND ( 'NONE', #13006, .T. ) ;
#14785 =( GEOMETRIC_REPRESENTATION_CONTEXT ( 3 ) GLOBAL_UNCERTAINTY_ASSIGNED_CONTEXT ( ( #567 ) ) GLOBAL_UNIT_ASSIGNED_CONTEXT ( ( #7702, #5357, #727 ) ) REPRESENTATION_CONTEXT ( 'NONE', 'WORKASPACE' ) );
#14786 = DIRECTION ( 'NONE',  ( 1.000000000000000000, 0.000000000000000000, 0.000000000000000000 ) ) ;
#14787 = CARTESIAN_POINT ( 'NONE',  ( 0.000000000000000000, 1.178949249685215417, 2.042000000000002036 ) ) ;
#14788 = SURFACE_STYLE_USAGE ( .BOTH. , #10448 ) ;
#14789 = EDGE_CURVE ( 'NONE', #6138, #1696, #4620, .T. ) ;
#14790 = CARTESIAN_POINT ( 'NONE',  ( -29.49928053175900899, -45.83364790889059037, -13.00000000000000178 ) ) ;
#14791 = CIRCLE ( 'NONE', #12357, 50.00000000000000000 ) ;
#14792 = EDGE_CURVE ( 'NONE', #6859, #1107, #2962, .T. ) ;
#14793 = CARTESIAN_POINT ( 'NONE',  ( 89.33979373934423052, -36.70371619500547666, -10.50000000000000000 ) ) ;
#14794 = DIRECTION ( 'NONE',  ( 1.000000000000000000, 8.521448653921158262E-16, 0.000000000000000000 ) ) ;
#14795 = VERTEX_POINT ( 'NONE', #14662 ) ;
#14796 = ORIENTED_EDGE ( 'NONE', *, *, #5737, .T. ) ;
#14797 = CARTESIAN_POINT ( 'NONE',  ( -18.52941176470586981, 60.21346111671361001, 31.00000000000000000 ) ) ;
#14798 = ORIENTED_EDGE ( 'NONE', *, *, #9125, .T. ) ;
#14799 = CIRCLE ( 'NONE', #9927, 100.0000000000000000 ) ;
#14800 = ORIENTED_EDGE ( 'NONE', *, *, #3671, .F. ) ;
#14801 = CARTESIAN_POINT ( 'NONE',  ( 0.000000000000000000, 0.000000000000000000, 8.000000000000000000 ) ) ;
#14802 = AXIS2_PLACEMENT_3D ( 'NONE', #3308, #7700, #9141 ) ;
#14803 = AXIS2_PLACEMENT_3D ( 'NONE', #6010, #250, #9505 ) ;
#14804 = CIRCLE ( 'NONE', #1705, 59.49999999999999289 ) ;
#14805 = EDGE_CURVE ( 'NONE', #1282, #13160, #13830, .T. ) ;
#14806 = DIRECTION ( 'NONE',  ( 1.000000000000000000, 0.000000000000000000, 0.000000000000000000 ) ) ;
#14807 = CARTESIAN_POINT ( 'NONE',  ( -69.08004447556112382, -68.68541276968802833, 10.49999999999999822 ) ) ;
#14808 = CARTESIAN_POINT ( 'NONE',  ( -3.492805317593278058, 46.55633131742322917, -13.00000000000000178 ) ) ;
#14809 = DIRECTION ( 'NONE',  ( -1.000000000000000000, 0.000000000000000000, 0.000000000000000000 ) ) ;
#14810 = EDGE_CURVE ( 'NONE', #12421, #8030, #13576, .T. ) ;
#14811 = VECTOR ( 'NONE', #5023, 1000.000000000000000 ) ;
#14812 = PLANE ( 'NONE',  #973 ) ;
#14813 = ORIENTED_EDGE ( 'NONE', *, *, #11022, .F. ) ;
#14814 = CARTESIAN_POINT ( 'NONE',  ( 70.71067811865438557, -70.71067811865511032, 8.000000000000000000 ) ) ;
#14815 = AXIS2_PLACEMENT_3D ( 'NONE', #696, #3123, #626 ) ;
#14816 = CIRCLE ( 'NONE', #9452, 52.50000000000000711 ) ;
#14817 = CARTESIAN_POINT ( 'NONE',  ( 32.46576781417953583, -41.59008834022656487, 10.49999999999999822 ) ) ;
#14818 = CARTESIAN_POINT ( 'NONE',  ( -1.391697335622808396, -4.043246145443389672, -3.503898532754371242 ) ) ;
#14819 = VERTEX_POINT ( 'NONE', #7664 ) ;
#14820 = DIRECTION ( 'NONE',  ( -1.000000000000000000, 1.224646799147352714E-16, 0.000000000000000000 ) ) ;
#14821 = AXIS2_PLACEMENT_3D ( 'NONE', #2499, #4786, #7117 ) ;
#14822 = AXIS2_PLACEMENT_3D ( 'NONE', #11620, #4777, #3491 ) ;
#14823 = CARTESIAN_POINT ( 'NONE',  ( -36.14014761921588104, 11.74264578624790190, -25.50000000000000355 ) ) ;
#14824 = DIRECTION ( 'NONE',  ( 1.000000000000000000, 0.000000000000000000, 0.000000000000000000 ) ) ;
#14825 = VECTOR ( 'NONE', #12805, 1000.000000000000000 ) ;
#14826 = AXIS2_PLACEMENT_3D ( 'NONE', #5012, #442, #3866 ) ;
#14827 = CARTESIAN_POINT ( 'NONE',  ( -12.07539369549097863, 94.22990561005788379, -17.09692597381455315 ) ) ;
#14828 = CARTESIAN_POINT ( 'NONE',  ( -33.48561063518626923, 47.21331623427104063, -13.00000000000000178 ) ) ;
#14829 = CARTESIAN_POINT ( 'NONE',  ( 53.63365512954693770, -9.714003807513686084, 8.000000000000000000 ) ) ;
#14830 = DIRECTION ( 'NONE',  ( -0.000000000000000000, -0.000000000000000000, -1.000000000000000000 ) ) ;
#14831 = CARTESIAN_POINT ( 'NONE',  ( 12.50000000000000000, 40.62019202317980415, 31.00000000000000000 ) ) ;
#14832 = DIRECTION ( 'NONE',  ( 1.000000000000000000, -1.826024711554534012E-15, 0.000000000000000000 ) ) ;
#14833 = EDGE_CURVE ( 'NONE', #9386, #1607, #6438, .T. ) ;
#14834 = AXIS2_PLACEMENT_3D ( 'NONE', #8670, #5114, #10958 ) ;
#14835 = ORIENTED_EDGE ( 'NONE', *, *, #1702, .F. ) ;
#14836 = EDGE_CURVE ( 'NONE', #13552, #3890, #11090, .T. ) ;
#14837 = CARTESIAN_POINT ( 'NONE',  ( 13.71740939043365337, -51.19406879332061067, 8.000000000000000000 ) ) ;
#14838 = DIRECTION ( 'NONE',  ( 0.000000000000000000, 0.000000000000000000, 1.000000000000000000 ) ) ;
#14839 = AXIS2_PLACEMENT_3D ( 'NONE', #4663, #4810, #14148 ) ;
#14840 = CARTESIAN_POINT ( 'NONE',  ( -89.61631465359441506, 37.12029293941468211, -8.000000000000000000 ) ) ;
#14841 = PRODUCT_DEFINITION_SHAPE ( 'NONE', 'NONE',  #420 ) ;
#14842 = DIRECTION ( 'NONE',  ( 1.000000000000000000, 0.000000000000000000, 0.000000000000000000 ) ) ;
#14843 = ORIENTED_EDGE ( 'NONE', *, *, #844, .T. ) ;
#14844 = EDGE_CURVE ( 'NONE', #10355, #4159, #9931, .T. ) ;
#14845 = CARTESIAN_POINT ( 'NONE',  ( 29.49928053175900899, 45.83364790889059037, 8.000000000000000000 ) ) ;
#14846 = ORIENTED_EDGE ( 'NONE', *, *, #10049, .T. ) ;
#14847 = AXIS2_PLACEMENT_3D ( 'NONE', #871, #14689, #6534 ) ;
#14848 = DIRECTION ( 'NONE',  ( 1.000000000000000000, 0.000000000000000000, 0.000000000000000000 ) ) ;
#14849 = DIRECTION ( 'NONE',  ( 0.000000000000000000, 0.000000000000000000, -1.000000000000000000 ) ) ;
#14850 = DIRECTION ( 'NONE',  ( 0.000000000000000000, 0.000000000000000000, 1.000000000000000000 ) ) ;
#14851 = AXIS2_PLACEMENT_3D ( 'NONE', #13545, #6626, #10201 ) ;
#14852 = CARTESIAN_POINT ( 'NONE',  ( -37.12029293941441210, -89.61631465359452875, -10.50000000000000000 ) ) ;
#14853 = ORIENTED_EDGE ( 'NONE', *, *, #5473, .F. ) ;
#14854 = ORIENTED_EDGE ( 'NONE', *, *, #11259, .T. ) ;
#14855 = EDGE_LOOP ( 'NONE', ( #4520, #13489 ) ) ;
#14856 = EDGE_CURVE ( 'NONE', #1115, #13227, #767, .T. ) ;
#14857 = DIRECTION ( 'NONE',  ( -1.000000000000000000, 0.000000000000000000, 0.000000000000000000 ) ) ;
#14858 = CARTESIAN_POINT ( 'NONE',  ( 34.65532077583679893, 101.0090414146251590, 15.74457401924681932 ) ) ;
#14859 = CIRCLE ( 'NONE', #8297, 0.5000000000000004441 ) ;
#14860 = DIRECTION ( 'NONE',  ( 1.000000000000000000, 0.000000000000000000, 0.000000000000000000 ) ) ;
#14861 = ORIENTED_EDGE ( 'NONE', *, *, #7259, .F. ) ;
#14862 = ORIENTED_EDGE ( 'NONE', *, *, #13873, .T. ) ;
#14863 = ORIENTED_EDGE ( 'NONE', *, *, #4469, .T. ) ;
#14864 = CARTESIAN_POINT ( 'NONE',  ( 12.05075418994416125, 74.02560756970278533, 17.09116503294089995 ) ) ;
#14865 = AXIS2_PLACEMENT_3D ( 'NONE', #14001, #12784, #3595 ) ;
#14866 = DIRECTION ( 'NONE',  ( -1.000000000000000000, 0.000000000000000000, 0.000000000000000000 ) ) ;
#14867 = DIRECTION ( 'NONE',  ( 1.000000000000000000, 0.000000000000000000, 0.000000000000000000 ) ) ;
#14868 = DIRECTION ( 'NONE',  ( -0.000000000000000000, -0.000000000000000000, -1.000000000000000000 ) ) ;
#14869 = ORIENTED_EDGE ( 'NONE', *, *, #11325, .T. ) ;
#14870 = CARTESIAN_POINT ( 'NONE',  ( -36.14014761921588104, 11.74264578624790190, -25.50000000000000355 ) ) ;
#14871 = ORIENTED_EDGE ( 'NONE', *, *, #363, .F. ) ;
#14872 = ORIENTED_EDGE ( 'NONE', *, *, #2922, .T. ) ;
#14873 = CARTESIAN_POINT ( 'NONE',  ( 25.00000000000000000, 81.24038404635960831, -16.00000000000000000 ) ) ;
#14874 = FACE_OUTER_BOUND ( 'NONE', #13512, .T. ) ;
#14875 = AXIS2_PLACEMENT_3D ( 'NONE', #10304, #9083, #1132 ) ;
#14876 = ORIENTED_EDGE ( 'NONE', *, *, #13497, .F. ) ;
#14877 = CIRCLE ( 'NONE', #9768, 0.5000000000000004441 ) ;
#14878 = VERTEX_POINT ( 'NONE', #3191 ) ;
#14879 = CARTESIAN_POINT ( 'NONE',  ( 9.917888187663120192, 52.54657765281190507, 8.000000000000000000 ) ) ;
#14880 = EDGE_CURVE ( 'NONE', #13797, #9064, #1941, .T. ) ;
#14881 = VERTEX_POINT ( 'NONE', #13287 ) ;
#14882 = ORIENTED_EDGE ( 'NONE', *, *, #13042, .F. ) ;
#14883 = CARTESIAN_POINT ( 'NONE',  ( -37.02125851216292318, 90.10640870805768543, -13.00000000000000178 ) ) ;
#14884 = DIRECTION ( 'NONE',  ( 1.000000000000000000, 0.000000000000000000, 0.000000000000000000 ) ) ;
#14885 = AXIS2_PLACEMENT_3D ( 'NONE', #2926, #1793, #6401 ) ;
#14886 = DIRECTION ( 'NONE',  ( 0.000000000000000000, 0.000000000000000000, 1.000000000000000000 ) ) ;
#14887 = CYLINDRICAL_SURFACE ( 'NONE', #12, 0.5000000000000004441 ) ;
#14888 = CARTESIAN_POINT ( 'NONE',  ( 45.88839665196118744, -26.99988008862642630, 10.49999999999999822 ) ) ;
#14889 = AXIS2_PLACEMENT_3D ( 'NONE', #8690, #8775, #10069 ) ;
#14890 = ORIENTED_EDGE ( 'NONE', *, *, #5567, .T. ) ;
#14891 = DIRECTION ( 'NONE',  ( -1.000000000000000000, -0.000000000000000000, -0.000000000000000000 ) ) ;
#14892 = ORIENTED_EDGE ( 'NONE', *, *, #2845, .F. ) ;
#14893 = AXIS2_PLACEMENT_3D ( 'NONE', #9337, #3430, #12546 ) ;
#14894 = DIRECTION ( 'NONE',  ( -1.000000000000000000, -3.552713678800500929E-15, 0.000000000000000000 ) ) ;
#14895 = CARTESIAN_POINT ( 'NONE',  ( 0.000000000000000000, 0.000000000000000000, 10.50000000000000000 ) ) ;
#14896 = CIRCLE ( 'NONE', #13434, 0.5000000000000022204 ) ;
#14897 = ADVANCED_FACE ( 'NONE', ( #618 ), #5830, .T. ) ;
#14898 = VERTEX_POINT ( 'NONE', #8187 ) ;
#14899 = CARTESIAN_POINT ( 'NONE',  ( 2.059999999999998721, 0.000000000000000000, -0.3080913168122742518 ) ) ;
#14900 = ADVANCED_FACE ( 'NONE', ( #13820 ), #10469, .T. ) ;
#14901 = EDGE_CURVE ( 'NONE', #14021, #12633, #12624, .T. ) ;
#14902 = LINE ( 'NONE', #1523, #9782 ) ;
#14903 = DIRECTION ( 'NONE',  ( 0.000000000000000000, 0.000000000000000000, -1.000000000000000000 ) ) ;
#14904 = AXIS2_PLACEMENT_3D ( 'NONE', #1100, #5779, #170 ) ;
#14905 = CARTESIAN_POINT ( 'NONE',  ( -27.00670028307162340, -46.24878538001323136, -10.50000000000000000 ) ) ;
#14906 = DIRECTION ( 'NONE',  ( 0.000000000000000000, 0.000000000000000000, -1.000000000000000000 ) ) ;
#14907 = DIRECTION ( 'NONE',  ( 0.2941176470588238168, -0.9557692240748187906, 0.000000000000000000 ) ) ;
#14908 = AXIS2_PLACEMENT_3D ( 'NONE', #8353, #1301, #10706 ) ;
#14909 = AXIS2_PLACEMENT_3D ( 'NONE', #438, #13202, #6040 ) ;
#14910 = DIRECTION ( 'NONE',  ( 1.000000000000000000, 0.000000000000000000, 0.000000000000000000 ) ) ;
#14911 =( NAMED_UNIT ( * ) SI_UNIT ( $, .STERADIAN. ) SOLID_ANGLE_UNIT ( ) );
#14912 = ORIENTED_EDGE ( 'NONE', *, *, #7118, .F. ) ;
#14913 = FACE_BOUND ( 'NONE', #8657, .T. ) ;
#14914 = CARTESIAN_POINT ( 'NONE',  ( -53.26842454702436669, -11.55014193876159645, -13.00000000000000178 ) ) ;
#14915 = CIRCLE ( 'NONE', #3741, 0.5000000000000004441 ) ;
#14916 = CARTESIAN_POINT ( 'NONE',  ( 9.706953719245472456, 57.06275842387054098, 10.49999999999999822 ) ) ;
#14917 = CIRCLE ( 'NONE', #8360, 3.000000000000002665 ) ;
#14918 = CIRCLE ( 'NONE', #12972, 20.00000000000000000 ) ;
#14919 = AXIS2_PLACEMENT_3D ( 'NONE', #6106, #554, #8235 ) ;
#14920 = CARTESIAN_POINT ( 'NONE',  ( -6.917888187662729393, -52.54657765281195481, 10.49999999999999822 ) ) ;
#14921 = ORIENTED_EDGE ( 'NONE', *, *, #142, .F. ) ;
#14922 = DIRECTION ( 'NONE',  ( 0.000000000000000000, 0.000000000000000000, 1.000000000000000000 ) ) ;
#14923 = EDGE_LOOP ( 'NONE', ( #3689, #5880, #14548, #1973, #8659, #13727, #13014, #13968, #4456 ) ) ;
#14924 = ADVANCED_FACE ( 'NONE', ( #9252 ), #14887, .F. ) ;
#14925 = CARTESIAN_POINT ( 'NONE',  ( -42.04772703543551415, -32.26435573746212526, -13.00000000000000178 ) ) ;
#14926 =( NAMED_UNIT ( * ) PLANE_ANGLE_UNIT ( ) SI_UNIT ( $, .RADIAN. ) );
#14927 = CIRCLE ( 'NONE', #13967, 59.50000000000000000 ) ;
#14928 = ADVANCED_FACE ( 'NONE', ( #11392 ), #9693, .T. ) ;
#14929 = CYLINDRICAL_SURFACE ( 'NONE', #4613, 59.50000000000000000 ) ;
#14930 = CARTESIAN_POINT ( 'NONE',  ( -36.52608637591512775, 92.55687898036946137, -8.000000000000000000 ) ) ;
#14931 = VERTEX_POINT ( 'NONE', #11623 ) ;
#14932 = AXIS2_PLACEMENT_3D ( 'NONE', #14738, #7729, #8875 ) ;
#14933 = VERTEX_POINT ( 'NONE', #11475 ) ;
#14934 = VERTEX_POINT ( 'NONE', #2277 ) ;
#14935 = CARTESIAN_POINT ( 'NONE',  ( -32.46576781417928714, 41.59008834022678514, 10.49999999999999822 ) ) ;
#14936 = DIRECTION ( 'NONE',  ( 0.000000000000000000, 0.000000000000000000, 1.000000000000000000 ) ) ;
#14937 = DIRECTION ( 'NONE',  ( 0.000000000000000000, 0.000000000000000000, -1.000000000000000000 ) ) ;
#14938 = AXIS2_PLACEMENT_3D ( 'NONE', #3008, #814, #14711 ) ;
#14939 = VERTEX_POINT ( 'NONE', #5611 ) ;
#14940 = VERTEX_POINT ( 'NONE', #1148 ) ;
#14941 = ADVANCED_FACE ( 'NONE', ( #9106 ), #6894, .F. ) ;
#14942 = EDGE_LOOP ( 'NONE', ( #6029, #11944, #435, #10461 ) ) ;
#14943 = ADVANCED_FACE ( 'NONE', ( #3266 ), #1325, .F. ) ;
#14944 = DIRECTION ( 'NONE',  ( -1.000000000000000000, 0.000000000000000000, 0.000000000000000000 ) ) ;
#14945 = DIRECTION ( 'NONE',  ( -1.000000000000000000, 0.000000000000000000, 0.000000000000000000 ) ) ;
#14946 = CARTESIAN_POINT ( 'NONE',  ( 0.000000000000000000, 0.000000000000000000, 31.00000000000000000 ) ) ;
#14947 = DIRECTION ( 'NONE',  ( -0.000000000000000000, -0.000000000000000000, -1.000000000000000000 ) ) ;
#14948 = VECTOR ( 'NONE', #8002, 1000.000000000000114 ) ;
#14949 = ORIENTED_EDGE ( 'NONE', *, *, #7350, .T. ) ;
#14950 = FACE_OUTER_BOUND ( 'NONE', #3321, .T. ) ;
#14951 = ORIENTED_EDGE ( 'NONE', *, *, #125, .F. ) ;
#14952 = EDGE_CURVE ( 'NONE', #5997, #11991, #8724, .T. ) ;
#14953 = LINE ( 'NONE', #4549, #5200 ) ;
#14954 = LINE ( 'NONE', #14797, #10128 ) ;
#14955 = ORIENTED_EDGE ( 'NONE', *, *, #9964, .T. ) ;
#14956 = VERTEX_POINT ( 'NONE', #5539 ) ;
#14957 = CARTESIAN_POINT ( 'NONE',  ( 0.000000000000000000, 0.000000000000000000, 0.000000000000000000 ) ) ;
#14958 = AXIS2_PLACEMENT_3D ( 'NONE', #4274, #6512, #1899 ) ;
#14959 = EDGE_LOOP ( 'NONE', ( #9925, #10814, #6373, #1313, #14654 ) ) ;
#14960 = EDGE_CURVE ( 'NONE', #669, #215, #8257, .T. ) ;
#14961 = VERTEX_POINT ( 'NONE', #4415 ) ;
#14962 = CARTESIAN_POINT ( 'NONE',  ( -69.16568774265545017, 71.53347797788843820, 8.000000000000000000 ) ) ;
#14963 = DIRECTION ( 'NONE',  ( -1.000000000000000000, 0.000000000000000000, 0.000000000000000000 ) ) ;
#14964 = DIRECTION ( 'NONE',  ( 1.000000000000000000, 0.000000000000000000, 0.000000000000000000 ) ) ;
#14965 = DIRECTION ( 'NONE',  ( -0.000000000000000000, -0.000000000000000000, 1.000000000000000000 ) ) ;
#14966 = VECTOR ( 'NONE', #4321, 1000.000000000000000 ) ;
#14967 = CARTESIAN_POINT ( 'NONE',  ( 0.000000000000000000, 0.000000000000000000, -25.50000000000000355 ) ) ;
#14968 = ORIENTED_EDGE ( 'NONE', *, *, #2587, .T. ) ;
#14969 = AXIS2_PLACEMENT_3D ( 'NONE', #1758, #8655, #2826 ) ;
#14970 = DIRECTION ( 'NONE',  ( -0.000000000000000000, -0.000000000000000000, -1.000000000000000000 ) ) ;
#14971 = EDGE_CURVE ( 'NONE', #5320, #9151, #10671, .T. ) ;
#14972 = FACE_OUTER_BOUND ( 'NONE', #13747, .T. ) ;
#14973 = ORIENTED_EDGE ( 'NONE', *, *, #11937, .F. ) ;
#14974 = DIRECTION ( 'NONE',  ( 0.000000000000000000, 0.000000000000000000, 1.000000000000000000 ) ) ;
#14975 = DIRECTION ( 'NONE',  ( 1.000000000000000000, 0.000000000000000000, 0.000000000000000000 ) ) ;
#14976 = ORIENTED_EDGE ( 'NONE', *, *, #7922, .F. ) ;
#14977 = DIRECTION ( 'NONE',  ( -0.000000000000000000, -0.000000000000000000, -1.000000000000000000 ) ) ;
#14978 = CYLINDRICAL_SURFACE ( 'NONE', #13957, 59.50000000000000000 ) ;
#14979 = LINE ( 'NONE', #12620, #13354 ) ;
#14980 = DIRECTION ( 'NONE',  ( 0.000000000000000000, 0.000000000000000000, 1.000000000000000000 ) ) ;
#14981 = ADVANCED_FACE ( 'NONE', ( #6736 ), #10841, .F. ) ;
#14982 = LINE ( 'NONE', #4576, #8220 ) ;
#14983 = ADVANCED_FACE ( 'NONE', ( #7339 ), #14566, .F. ) ;
#14984 = EDGE_CURVE ( 'NONE', #4528, #27, #11667, .T. ) ;
#14985 = FACE_OUTER_BOUND ( 'NONE', #1175, .T. ) ;
#14986 = ORIENTED_EDGE ( 'NONE', *, *, #9427, .F. ) ;
#14987 = DIRECTION ( 'NONE',  ( -0.000000000000000000, -0.000000000000000000, 1.000000000000000000 ) ) ;
#14988 = CARTESIAN_POINT ( 'NONE',  ( 0.000000000000000000, 0.000000000000000000, -4.974599999999998801 ) ) ;
#14989 = CIRCLE ( 'NONE', #8428, 100.0000000000000000 ) ;
#14990 = PLANE ( 'NONE',  #11967 ) ;
#14991 = EDGE_CURVE ( 'NONE', #12263, #11561, #8416, .T. ) ;
#14992 = DIRECTION ( 'NONE',  ( 1.000000000000000000, 0.000000000000000000, -0.000000000000000000 ) ) ;
#14993 = ORIENTED_EDGE ( 'NONE', *, *, #14960, .F. ) ;
#14994 = CARTESIAN_POINT ( 'NONE',  ( -57.06275842387042729, 9.706953719246069312, -13.00000000000000178 ) ) ;
#14995 = ORIENTED_EDGE ( 'NONE', *, *, #1110, .F. ) ;
#14996 = ADVANCED_FACE ( 'NONE', ( #3863 ), #8480, .T. ) ;
#14997 = CARTESIAN_POINT ( 'NONE',  ( 97.00000000000000000, -3.384287605079545030E-13, 10.49999999999999822 ) ) ;
#14998 = CARTESIAN_POINT ( 'NONE',  ( -3.999999999999996447, 0.000000000000000000, 0.000000000000000000 ) ) ;
#14999 = AXIS2_PLACEMENT_3D ( 'NONE', #13330, #8773, #10983 ) ;
#15000 = CARTESIAN_POINT ( 'NONE',  ( 0.000000000000000000, 0.000000000000000000, -10.50000000000000000 ) ) ;
#15001 = CARTESIAN_POINT ( 'NONE',  ( 100.0000000000000000, -1.224646799147353217E-14, -13.00000000000000178 ) ) ;
#15002 = ORIENTED_EDGE ( 'NONE', *, *, #12141, .F. ) ;
#15003 = EDGE_CURVE ( 'NONE', #9892, #2714, #14816, .T. ) ;
#15004 = ORIENTED_EDGE ( 'NONE', *, *, #6971, .T. ) ;
#15005 = ORIENTED_EDGE ( 'NONE', *, *, #10424, .F. ) ;
#15006 = DIRECTION ( 'NONE',  ( 1.000000000000000000, 0.000000000000000000, 0.000000000000000000 ) ) ;
#15007 = DIRECTION ( 'NONE',  ( 0.000000000000000000, 0.000000000000000000, 1.000000000000000000 ) ) ;
#15008 = DIRECTION ( 'NONE',  ( 0.000000000000000000, 0.000000000000000000, 1.000000000000000000 ) ) ;
#15009 = ORIENTED_EDGE ( 'NONE', *, *, #12386, .F. ) ;
#15010 = EDGE_LOOP ( 'NONE', ( #752, #11481, #7344, #4868 ) ) ;
#15011 = VERTEX_POINT ( 'NONE', #1588 ) ;
#15012 = CARTESIAN_POINT ( 'NONE',  ( 12.26010588040893978, 73.99122283359872654, 16.55683232866783783 ) ) ;
#15013 = DIRECTION ( 'NONE',  ( -0.000000000000000000, -0.000000000000000000, -1.000000000000000000 ) ) ;
#15014 = CARTESIAN_POINT ( 'NONE',  ( -2.449293598294708880E-16, 38.00000000000000000, 14.49999999999999822 ) ) ;
#15015 = CYLINDRICAL_SURFACE ( 'NONE', #13492, 0.5000000000000073275 ) ;
#15016 = DIRECTION ( 'NONE',  ( -0.000000000000000000, -0.000000000000000000, -1.000000000000000000 ) ) ;
#15017 = ORIENTED_EDGE ( 'NONE', *, *, #12606, .T. ) ;
#15018 = DIRECTION ( 'NONE',  ( 0.000000000000000000, 0.000000000000000000, 1.000000000000000000 ) ) ;
#15019 = AXIS2_PLACEMENT_3D ( 'NONE', #10410, #166, #12778 ) ;
#15021 = EDGE_CURVE ( 'NONE', #2772, #10943, #5825, .T. ) ;
#15020 = DIRECTION ( 'NONE',  ( -0.9557692240748189016, 0.2941176470588239833, 0.000000000000000000 ) ) ;
#15022 = EDGE_CURVE ( 'NONE', #4198, #12536, #1231, .T. ) ;
#15023 = ORIENTED_EDGE ( 'NONE', *, *, #8905, .T. ) ;
#15024 = VERTEX_POINT ( 'NONE', #2643 ) ;
#15025 = CARTESIAN_POINT ( 'NONE',  ( -4.000000000000000888, 2.309401076758495375, -3.504269196027867128 ) ) ;
#15026 =( GEOMETRIC_REPRESENTATION_CONTEXT ( 3 ) GLOBAL_UNCERTAINTY_ASSIGNED_CONTEXT ( ( #1700 ) ) GLOBAL_UNIT_ASSIGNED_CONTEXT ( ( #4612, #9157, #13648 ) ) REPRESENTATION_CONTEXT ( 'NONE', 'WORKASPACE' ) );
#15027 = ORIENTED_EDGE ( 'NONE', *, *, #6655, .F. ) ;
#15028 = EDGE_LOOP ( 'NONE', ( #6398, #8836 ) ) ;
#15029 = DIRECTION ( 'NONE',  ( 0.000000000000000000, 0.000000000000000000, 1.000000000000000000 ) ) ;
#15030 = NEXT_ASSEMBLY_USAGE_OCCURRENCE ( 'NAUO1', ' ', ' ', #420, #898, $ ) ;
#15031 = NEXT_ASSEMBLY_USAGE_OCCURRENCE ( 'NAUO2', ' ', ' ', #420, #3579, $ ) ;
#15032 = NEXT_ASSEMBLY_USAGE_OCCURRENCE ( 'NAUO3', ' ', ' ', #420, #8937, $ ) ;
#15033 = NEXT_ASSEMBLY_USAGE_OCCURRENCE ( 'NAUO4', ' ', ' ', #420, #3850, $ ) ;
#15034 = NEXT_ASSEMBLY_USAGE_OCCURRENCE ( 'NAUO5', ' ', ' ', #420, #9593, $ ) ;
#15035 = NEXT_ASSEMBLY_USAGE_OCCURRENCE ( 'NAUO6', ' ', ' ', #420, #9593, $ ) ;
#15036 = NEXT_ASSEMBLY_USAGE_OCCURRENCE ( 'NAUO7', ' ', ' ', #420, #9593, $ ) ;
#15037 = NEXT_ASSEMBLY_USAGE_OCCURRENCE ( 'NAUO8', ' ', ' ', #420, #9593, $ ) ;
#15038 = NEXT_ASSEMBLY_USAGE_OCCURRENCE ( 'NAUO9', ' ', ' ', #420, #9593, $ ) ;
#15039 = NEXT_ASSEMBLY_USAGE_OCCURRENCE ( 'NAUO10', ' ', ' ', #420, #14333, $ ) ;
#15040 = NEXT_ASSEMBLY_USAGE_OCCURRENCE ( 'NAUO11', ' ', ' ', #420, #14333, $ ) ;
#15041 = NEXT_ASSEMBLY_USAGE_OCCURRENCE ( 'NAUO12', ' ', ' ', #420, #14333, $ ) ;
#15042 = NEXT_ASSEMBLY_USAGE_OCCURRENCE ( 'NAUO13', ' ', ' ', #420, #14333, $ ) ;
#15043 = NEXT_ASSEMBLY_USAGE_OCCURRENCE ( 'NAUO14', ' ', ' ', #420, #14333, $ ) ;
#15044 = NEXT_ASSEMBLY_USAGE_OCCURRENCE ( 'NAUO15', ' ', ' ', #420, #3579, $ ) ;
ENDSEC;
END-ISO-10303-21;
